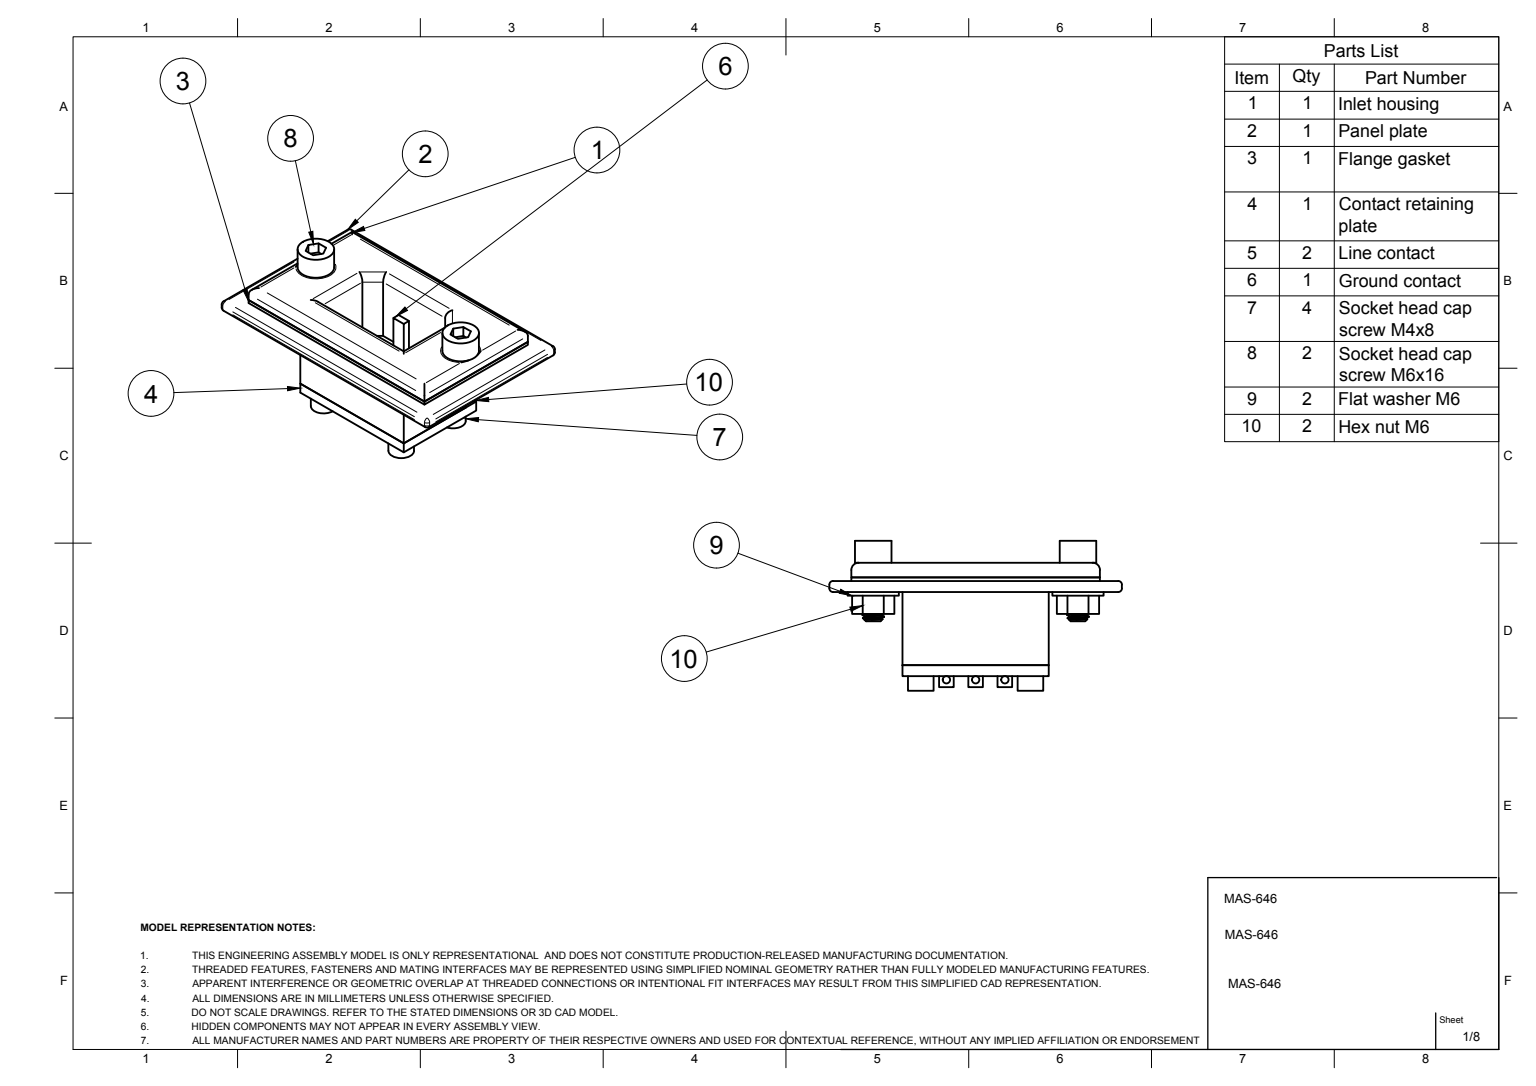
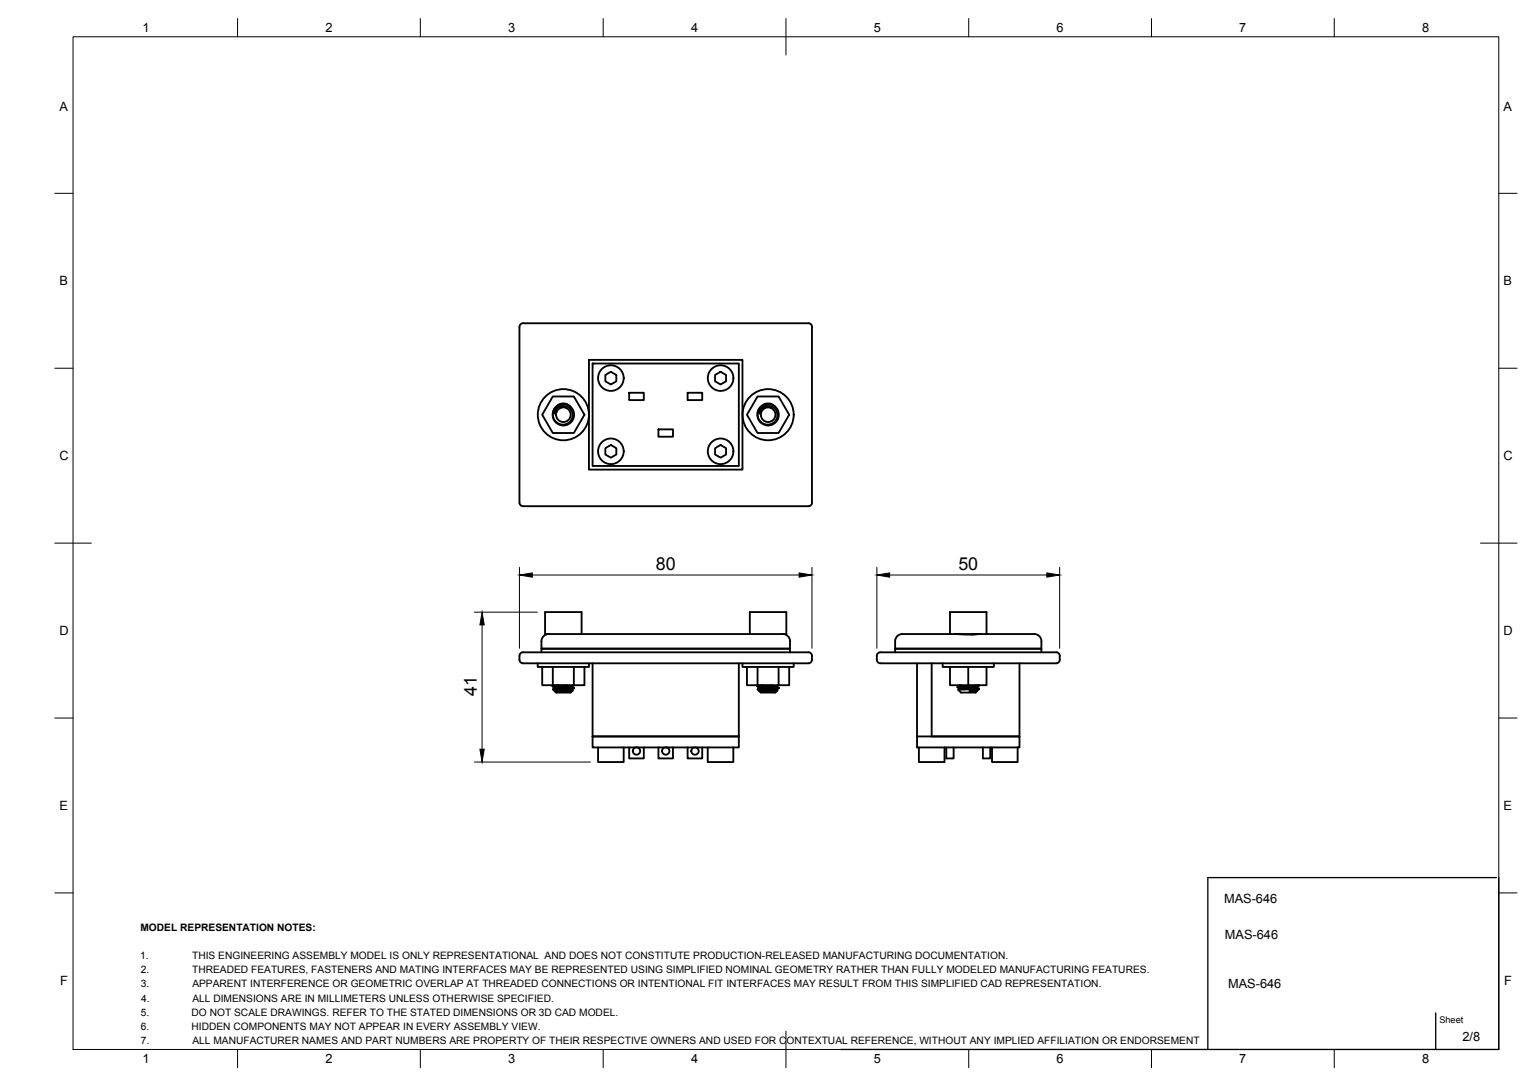
ISO-10303-21;
HEADER;
/* Generated by software containing ST-Developer
 * from STEP Tools, Inc. (www.steptools.com) 
 */

FILE_DESCRIPTION(
/* description */ ('Independent keyed three-contact power inlet for the IEC-connector des
ign category. Longer ground blade, retained contacts, wire termination
 holes and sealed bolted panel interface. Nominal custom interface; IE
C dimensional compatibility and electrical ratings are not assigned.'),

/* implementation_level */ '2;1');

FILE_NAME(
/* name */ 'MAS-646.step',
/* time_stamp */ '2026-11-08T19:55:04-08:00',
/* author */ (''),
/* organization */ (''),
/* preprocessor_version */ 'ST-DEVELOPER v20.2',
/* originating_system */ 'Autodesk Translation Framework v15.17.0.0',
/* authorisation */ '');

FILE_SCHEMA (('AUTOMOTIVE_DESIGN { 1 0 10303 214 3 1 1 }'));
ENDSEC;

DATA;
#10=MECHANICAL_DESIGN_GEOMETRIC_PRESENTATION_REPRESENTATION('',(#109,#110,
#111,#112,#113,#114,#115,#116,#117,#118),#21880);
#11=ITEM_DEFINED_TRANSFORMATION($,$,#6503,#6950);
#12=ITEM_DEFINED_TRANSFORMATION($,$,#6693,#6951);
#13=ITEM_DEFINED_TRANSFORMATION($,$,#6754,#6952);
#14=ITEM_DEFINED_TRANSFORMATION($,$,#6771,#6953);
#15=ITEM_DEFINED_TRANSFORMATION($,$,#6812,#6954);
#16=ITEM_DEFINED_TRANSFORMATION($,$,#6802,#6955);
#17=ITEM_DEFINED_TRANSFORMATION($,$,#6822,#6956);
#18=ITEM_DEFINED_TRANSFORMATION($,$,#6864,#6957);
#19=ITEM_DEFINED_TRANSFORMATION($,$,#6916,#6958);
#20=ITEM_DEFINED_TRANSFORMATION($,$,#6925,#6959);
#21=ITEM_DEFINED_TRANSFORMATION($,$,#6812,#6960);
#22=ITEM_DEFINED_TRANSFORMATION($,$,#6822,#6961);
#23=ITEM_DEFINED_TRANSFORMATION($,$,#6822,#6962);
#24=ITEM_DEFINED_TRANSFORMATION($,$,#6822,#6963);
#25=ITEM_DEFINED_TRANSFORMATION($,$,#6864,#6964);
#26=ITEM_DEFINED_TRANSFORMATION($,$,#6916,#6965);
#27=ITEM_DEFINED_TRANSFORMATION($,$,#6925,#6966);
#28=(
REPRESENTATION_RELATIONSHIP($,$,#21925,#21924)
REPRESENTATION_RELATIONSHIP_WITH_TRANSFORMATION(#11)
SHAPE_REPRESENTATION_RELATIONSHIP()
);
#29=(
REPRESENTATION_RELATIONSHIP($,$,#21926,#21924)
REPRESENTATION_RELATIONSHIP_WITH_TRANSFORMATION(#12)
SHAPE_REPRESENTATION_RELATIONSHIP()
);
#30=(
REPRESENTATION_RELATIONSHIP($,$,#21927,#21924)
REPRESENTATION_RELATIONSHIP_WITH_TRANSFORMATION(#13)
SHAPE_REPRESENTATION_RELATIONSHIP()
);
#31=(
REPRESENTATION_RELATIONSHIP($,$,#21928,#21924)
REPRESENTATION_RELATIONSHIP_WITH_TRANSFORMATION(#14)
SHAPE_REPRESENTATION_RELATIONSHIP()
);
#32=(
REPRESENTATION_RELATIONSHIP($,$,#21930,#21924)
REPRESENTATION_RELATIONSHIP_WITH_TRANSFORMATION(#15)
SHAPE_REPRESENTATION_RELATIONSHIP()
);
#33=(
REPRESENTATION_RELATIONSHIP($,$,#21929,#21924)
REPRESENTATION_RELATIONSHIP_WITH_TRANSFORMATION(#16)
SHAPE_REPRESENTATION_RELATIONSHIP()
);
#34=(
REPRESENTATION_RELATIONSHIP($,$,#21931,#21924)
REPRESENTATION_RELATIONSHIP_WITH_TRANSFORMATION(#17)
SHAPE_REPRESENTATION_RELATIONSHIP()
);
#35=(
REPRESENTATION_RELATIONSHIP($,$,#21932,#21924)
REPRESENTATION_RELATIONSHIP_WITH_TRANSFORMATION(#18)
SHAPE_REPRESENTATION_RELATIONSHIP()
);
#36=(
REPRESENTATION_RELATIONSHIP($,$,#21933,#21924)
REPRESENTATION_RELATIONSHIP_WITH_TRANSFORMATION(#19)
SHAPE_REPRESENTATION_RELATIONSHIP()
);
#37=(
REPRESENTATION_RELATIONSHIP($,$,#21934,#21924)
REPRESENTATION_RELATIONSHIP_WITH_TRANSFORMATION(#20)
SHAPE_REPRESENTATION_RELATIONSHIP()
);
#38=(
REPRESENTATION_RELATIONSHIP($,$,#21930,#21924)
REPRESENTATION_RELATIONSHIP_WITH_TRANSFORMATION(#21)
SHAPE_REPRESENTATION_RELATIONSHIP()
);
#39=(
REPRESENTATION_RELATIONSHIP($,$,#21931,#21924)
REPRESENTATION_RELATIONSHIP_WITH_TRANSFORMATION(#22)
SHAPE_REPRESENTATION_RELATIONSHIP()
);
#40=(
REPRESENTATION_RELATIONSHIP($,$,#21931,#21924)
REPRESENTATION_RELATIONSHIP_WITH_TRANSFORMATION(#23)
SHAPE_REPRESENTATION_RELATIONSHIP()
);
#41=(
REPRESENTATION_RELATIONSHIP($,$,#21931,#21924)
REPRESENTATION_RELATIONSHIP_WITH_TRANSFORMATION(#24)
SHAPE_REPRESENTATION_RELATIONSHIP()
);
#42=(
REPRESENTATION_RELATIONSHIP($,$,#21932,#21924)
REPRESENTATION_RELATIONSHIP_WITH_TRANSFORMATION(#25)
SHAPE_REPRESENTATION_RELATIONSHIP()
);
#43=(
REPRESENTATION_RELATIONSHIP($,$,#21933,#21924)
REPRESENTATION_RELATIONSHIP_WITH_TRANSFORMATION(#26)
SHAPE_REPRESENTATION_RELATIONSHIP()
);
#44=(
REPRESENTATION_RELATIONSHIP($,$,#21934,#21924)
REPRESENTATION_RELATIONSHIP_WITH_TRANSFORMATION(#27)
SHAPE_REPRESENTATION_RELATIONSHIP()
);
#45=CONTEXT_DEPENDENT_SHAPE_REPRESENTATION(#28,#21907);
#46=CONTEXT_DEPENDENT_SHAPE_REPRESENTATION(#29,#21908);
#47=CONTEXT_DEPENDENT_SHAPE_REPRESENTATION(#30,#21909);
#48=CONTEXT_DEPENDENT_SHAPE_REPRESENTATION(#31,#21910);
#49=CONTEXT_DEPENDENT_SHAPE_REPRESENTATION(#32,#21911);
#50=CONTEXT_DEPENDENT_SHAPE_REPRESENTATION(#33,#21912);
#51=CONTEXT_DEPENDENT_SHAPE_REPRESENTATION(#34,#21913);
#52=CONTEXT_DEPENDENT_SHAPE_REPRESENTATION(#35,#21914);
#53=CONTEXT_DEPENDENT_SHAPE_REPRESENTATION(#36,#21915);
#54=CONTEXT_DEPENDENT_SHAPE_REPRESENTATION(#37,#21916);
#55=CONTEXT_DEPENDENT_SHAPE_REPRESENTATION(#38,#21917);
#56=CONTEXT_DEPENDENT_SHAPE_REPRESENTATION(#39,#21918);
#57=CONTEXT_DEPENDENT_SHAPE_REPRESENTATION(#40,#21919);
#58=CONTEXT_DEPENDENT_SHAPE_REPRESENTATION(#41,#21920);
#59=CONTEXT_DEPENDENT_SHAPE_REPRESENTATION(#42,#21921);
#60=CONTEXT_DEPENDENT_SHAPE_REPRESENTATION(#43,#21922);
#61=CONTEXT_DEPENDENT_SHAPE_REPRESENTATION(#44,#21923);
#62=NEXT_ASSEMBLY_USAGE_OCCURRENCE('Inlet housing:1','Inlet housing:1',
'Inlet housing:1',#21936,#21937,'Inlet housing:1');
#63=NEXT_ASSEMBLY_USAGE_OCCURRENCE('Panel plate:1','Panel plate:1',
'Panel plate:1',#21936,#21938,'Panel plate:1');
#64=NEXT_ASSEMBLY_USAGE_OCCURRENCE('Flange gasket:1','Flange gasket:1',
'Flange gasket:1',#21936,#21939,'Flange gasket:1');
#65=NEXT_ASSEMBLY_USAGE_OCCURRENCE('Contact retaining plate:1',
'Contact retaining plate:1','Contact retaining plate:1',#21936,#21940,
'Contact retaining plate:1');
#66=NEXT_ASSEMBLY_USAGE_OCCURRENCE('Line contact:1','Line contact:1',
'Line contact:1',#21936,#21942,'Line contact:1');
#67=NEXT_ASSEMBLY_USAGE_OCCURRENCE('Ground contact:1',
'Ground contact:1','Ground contact:1',#21936,#21941,'Ground contact:1');
#68=NEXT_ASSEMBLY_USAGE_OCCURRENCE('Socket head cap screw M4x8:1',
'Socket head cap screw M4x8:1','Socket head cap screw M4x8:1',#21936,#21943,
'Socket head cap screw M4x8:1');
#69=NEXT_ASSEMBLY_USAGE_OCCURRENCE('Socket head cap screw M6x16:1',
'Socket head cap screw M6x16:1','Socket head cap screw M6x16:1',#21936,
#21944,'Socket head cap screw M6x16:1');
#70=NEXT_ASSEMBLY_USAGE_OCCURRENCE('Flat washer M6:1',
'Flat washer M6:1','Flat washer M6:1',#21936,#21945,'Flat washer M6:1');
#71=NEXT_ASSEMBLY_USAGE_OCCURRENCE('Hex nut M6:1','Hex nut M6:1',
'Hex nut M6:1',#21936,#21946,'Hex nut M6:1');
#72=NEXT_ASSEMBLY_USAGE_OCCURRENCE('Line contact:2','Line contact:2',
'Line contact:2',#21936,#21942,'Line contact:2');
#73=NEXT_ASSEMBLY_USAGE_OCCURRENCE('Socket head cap screw M4x8:2',
'Socket head cap screw M4x8:2','Socket head cap screw M4x8:2',#21936,#21943,
'Socket head cap screw M4x8:2');
#74=NEXT_ASSEMBLY_USAGE_OCCURRENCE('Socket head cap screw M4x8:3',
'Socket head cap screw M4x8:3','Socket head cap screw M4x8:3',#21936,#21943,
'Socket head cap screw M4x8:3');
#75=NEXT_ASSEMBLY_USAGE_OCCURRENCE('Socket head cap screw M4x8:4',
'Socket head cap screw M4x8:4','Socket head cap screw M4x8:4',#21936,#21943,
'Socket head cap screw M4x8:4');
#76=NEXT_ASSEMBLY_USAGE_OCCURRENCE('Socket head cap screw M6x16:2',
'Socket head cap screw M6x16:2','Socket head cap screw M6x16:2',#21936,
#21944,'Socket head cap screw M6x16:2');
#77=NEXT_ASSEMBLY_USAGE_OCCURRENCE('Flat washer M6:2',
'Flat washer M6:2','Flat washer M6:2',#21936,#21945,'Flat washer M6:2');
#78=NEXT_ASSEMBLY_USAGE_OCCURRENCE('Hex nut M6:2','Hex nut M6:2',
'Hex nut M6:2',#21936,#21946,'Hex nut M6:2');
#79=CONICAL_SURFACE('',#6845,1.5,0.785398163397448);
#80=CONICAL_SURFACE('',#6897,2.5,0.785398163397448);
#81=SPHERICAL_SURFACE('',#6694,0.999999999999996);
#82=SPHERICAL_SURFACE('',#6698,0.999999999999996);
#83=SPHERICAL_SURFACE('',#6702,1.);
#84=SPHERICAL_SURFACE('',#6706,0.999999999999996);
#85=SPHERICAL_SURFACE('',#6710,1.);
#86=SPHERICAL_SURFACE('',#6714,0.999999999999996);
#87=SPHERICAL_SURFACE('',#6718,1.);
#88=SPHERICAL_SURFACE('',#6722,1.);
#89=SHAPE_REPRESENTATION_RELATIONSHIP('SRR','None',#21925,#99);
#90=SHAPE_REPRESENTATION_RELATIONSHIP('SRR','None',#21926,#100);
#91=SHAPE_REPRESENTATION_RELATIONSHIP('SRR','None',#21927,#101);
#92=SHAPE_REPRESENTATION_RELATIONSHIP('SRR','None',#21928,#102);
#93=SHAPE_REPRESENTATION_RELATIONSHIP('SRR','None',#21929,#103);
#94=SHAPE_REPRESENTATION_RELATIONSHIP('SRR','None',#21930,#104);
#95=SHAPE_REPRESENTATION_RELATIONSHIP('SRR','None',#21931,#105);
#96=SHAPE_REPRESENTATION_RELATIONSHIP('SRR','None',#21932,#106);
#97=SHAPE_REPRESENTATION_RELATIONSHIP('SRR','None',#21933,#107);
#98=SHAPE_REPRESENTATION_RELATIONSHIP('SRR','None',#21934,#108);
#99=ADVANCED_BREP_SHAPE_REPRESENTATION('',(#119),#21870);
#100=ADVANCED_BREP_SHAPE_REPRESENTATION('',(#120),#21871);
#101=ADVANCED_BREP_SHAPE_REPRESENTATION('',(#121),#21872);
#102=ADVANCED_BREP_SHAPE_REPRESENTATION('',(#122),#21873);
#103=ADVANCED_BREP_SHAPE_REPRESENTATION('',(#123),#21874);
#104=ADVANCED_BREP_SHAPE_REPRESENTATION('',(#124),#21875);
#105=ADVANCED_BREP_SHAPE_REPRESENTATION('',(#125),#21876);
#106=ADVANCED_BREP_SHAPE_REPRESENTATION('',(#126),#21877);
#107=ADVANCED_BREP_SHAPE_REPRESENTATION('',(#127),#21878);
#108=ADVANCED_BREP_SHAPE_REPRESENTATION('',(#128),#21879);
#109=STYLED_ITEM('',(#21984),#119);
#110=STYLED_ITEM('',(#21985),#120);
#111=STYLED_ITEM('',(#21986),#121);
#112=STYLED_ITEM('',(#21987),#122);
#113=STYLED_ITEM('',(#21988),#123);
#114=STYLED_ITEM('',(#21988),#124);
#115=STYLED_ITEM('',(#21986),#125);
#116=STYLED_ITEM('',(#21986),#126);
#117=STYLED_ITEM('',(#21988),#127);
#118=STYLED_ITEM('',(#21985),#128);
#119=MANIFOLD_SOLID_BREP('Body1',#6381);
#120=MANIFOLD_SOLID_BREP('Body1',#6382);
#121=MANIFOLD_SOLID_BREP('Body1',#6383);
#122=MANIFOLD_SOLID_BREP('Body1',#6384);
#123=MANIFOLD_SOLID_BREP('Body1',#6385);
#124=MANIFOLD_SOLID_BREP('Body1',#6386);
#125=MANIFOLD_SOLID_BREP('Body1',#6387);
#126=MANIFOLD_SOLID_BREP('Body1',#6388);
#127=MANIFOLD_SOLID_BREP('Body1',#6389);
#128=MANIFOLD_SOLID_BREP('Body1',#6390);
#129=B_SPLINE_SURFACE_WITH_KNOTS('',3,3,((#11744,#11745,#11746,#11747,#11748,
#11749,#11750,#11751,#11752,#11753,#11754,#11755,#11756,#11757,#11758,#11759,
#11760,#11761,#11762,#11763,#11764,#11765,#11766,#11767,#11768,#11769,#11770,
#11771,#11772,#11773,#11774,#11775,#11776,#11777,#11778,#11779,#11780,#11781,
#11782,#11783,#11784,#11785,#11786,#11787,#11788,#11789,#11790,#11791,#11792,
#11793,#11794,#11795,#11796,#11797,#11798,#11799,#11800,#11801,#11802,#11803,
#11804,#11805,#11806,#11807,#11808,#11809,#11810,#11811,#11812,#11813,#11814,
#11815,#11816,#11817,#11818,#11819,#11820),(#11821,#11822,#11823,#11824,
#11825,#11826,#11827,#11828,#11829,#11830,#11831,#11832,#11833,#11834,#11835,
#11836,#11837,#11838,#11839,#11840,#11841,#11842,#11843,#11844,#11845,#11846,
#11847,#11848,#11849,#11850,#11851,#11852,#11853,#11854,#11855,#11856,#11857,
#11858,#11859,#11860,#11861,#11862,#11863,#11864,#11865,#11866,#11867,#11868,
#11869,#11870,#11871,#11872,#11873,#11874,#11875,#11876,#11877,#11878,#11879,
#11880,#11881,#11882,#11883,#11884,#11885,#11886,#11887,#11888,#11889,#11890,
#11891,#11892,#11893,#11894,#11895,#11896,#11897),(#11898,#11899,#11900,
#11901,#11902,#11903,#11904,#11905,#11906,#11907,#11908,#11909,#11910,#11911,
#11912,#11913,#11914,#11915,#11916,#11917,#11918,#11919,#11920,#11921,#11922,
#11923,#11924,#11925,#11926,#11927,#11928,#11929,#11930,#11931,#11932,#11933,
#11934,#11935,#11936,#11937,#11938,#11939,#11940,#11941,#11942,#11943,#11944,
#11945,#11946,#11947,#11948,#11949,#11950,#11951,#11952,#11953,#11954,#11955,
#11956,#11957,#11958,#11959,#11960,#11961,#11962,#11963,#11964,#11965,#11966,
#11967,#11968,#11969,#11970,#11971,#11972,#11973,#11974),(#11975,#11976,
#11977,#11978,#11979,#11980,#11981,#11982,#11983,#11984,#11985,#11986,#11987,
#11988,#11989,#11990,#11991,#11992,#11993,#11994,#11995,#11996,#11997,#11998,
#11999,#12000,#12001,#12002,#12003,#12004,#12005,#12006,#12007,#12008,#12009,
#12010,#12011,#12012,#12013,#12014,#12015,#12016,#12017,#12018,#12019,#12020,
#12021,#12022,#12023,#12024,#12025,#12026,#12027,#12028,#12029,#12030,#12031,
#12032,#12033,#12034,#12035,#12036,#12037,#12038,#12039,#12040,#12041,#12042,
#12043,#12044,#12045,#12046,#12047,#12048,#12049,#12050,#12051)),
 .UNSPECIFIED.,.F.,.F.,.F.,(4,4),(4,1,1,1,1,1,1,1,1,1,1,1,1,1,1,1,1,1,1,
1,1,1,1,1,1,1,1,1,1,1,1,1,1,1,1,1,1,1,1,1,1,1,1,1,1,1,1,1,1,1,1,1,1,1,1,
1,1,1,1,1,1,1,1,1,1,1,1,1,1,1,1,1,1,1,4),(0.,0.0448889834294934),(11.8615800042567,
12.859180611653,13.8567812190493,14.8543818264456,15.8519824338419,16.8495830412382,
17.8471836486345,18.8447842560309,19.8423848634272,20.8399854708235,21.8375860782198,
22.8351866856161,23.8327872930124,24.8303879004087,25.827988507805,26.8255891152013,
27.8231897225976,28.8207903299939,29.8183909373903,30.8159915447866,31.8135921521829,
32.8111927595792,33.8087933669755,34.8063939743718,35.8039945817681,36.8015951891644,
37.7991957965607,38.796796403957,39.7943970113533,40.7919976187497,41.789598226146,
42.7871988335423,43.7847994409386,44.7824000483349,45.7800006557312,46.7776012631275,
47.7752018705238,48.7728024779201,49.7704030853164,50.7680036927128,51.7656043001091,
52.7632049075054,53.7608055149017,54.758406122298,55.7560067296943,56.7536073370906,
57.7512079444869,58.7488085518832,59.7464091592795,60.7440097666758,61.7416103740722,
62.7392109814685,63.7368115888648,64.7344121962611,65.7320128036574,66.7296134110537,
67.72721401845,68.7248146258463,69.7224152332426,70.7200158406389,71.7176164480352,
72.7152170554316,73.7128176628279,74.7104182702242,75.7080188776205,76.7056194850168,
77.7032200924131,78.7008206998094,79.6984213072057,80.696021914602,81.6936225219983,
82.6912231293946,83.688823736791,84.6864243441873,85.6840249515836),
 .UNSPECIFIED.);
#130=B_SPLINE_SURFACE_WITH_KNOTS('',3,3,((#12248,#12249,#12250,#12251,#12252,
#12253,#12254,#12255,#12256,#12257,#12258,#12259,#12260,#12261,#12262,#12263,
#12264,#12265,#12266,#12267,#12268,#12269,#12270,#12271,#12272,#12273,#12274,
#12275,#12276,#12277,#12278,#12279,#12280,#12281,#12282,#12283,#12284,#12285,
#12286,#12287,#12288,#12289,#12290,#12291,#12292,#12293,#12294,#12295,#12296,
#12297,#12298,#12299,#12300,#12301,#12302,#12303,#12304,#12305,#12306,#12307,
#12308,#12309,#12310,#12311,#12312,#12313,#12314,#12315,#12316,#12317,#12318,
#12319,#12320,#12321,#12322,#12323,#12324),(#12325,#12326,#12327,#12328,
#12329,#12330,#12331,#12332,#12333,#12334,#12335,#12336,#12337,#12338,#12339,
#12340,#12341,#12342,#12343,#12344,#12345,#12346,#12347,#12348,#12349,#12350,
#12351,#12352,#12353,#12354,#12355,#12356,#12357,#12358,#12359,#12360,#12361,
#12362,#12363,#12364,#12365,#12366,#12367,#12368,#12369,#12370,#12371,#12372,
#12373,#12374,#12375,#12376,#12377,#12378,#12379,#12380,#12381,#12382,#12383,
#12384,#12385,#12386,#12387,#12388,#12389,#12390,#12391,#12392,#12393,#12394,
#12395,#12396,#12397,#12398,#12399,#12400,#12401),(#12402,#12403,#12404,
#12405,#12406,#12407,#12408,#12409,#12410,#12411,#12412,#12413,#12414,#12415,
#12416,#12417,#12418,#12419,#12420,#12421,#12422,#12423,#12424,#12425,#12426,
#12427,#12428,#12429,#12430,#12431,#12432,#12433,#12434,#12435,#12436,#12437,
#12438,#12439,#12440,#12441,#12442,#12443,#12444,#12445,#12446,#12447,#12448,
#12449,#12450,#12451,#12452,#12453,#12454,#12455,#12456,#12457,#12458,#12459,
#12460,#12461,#12462,#12463,#12464,#12465,#12466,#12467,#12468,#12469,#12470,
#12471,#12472,#12473,#12474,#12475,#12476,#12477,#12478),(#12479,#12480,
#12481,#12482,#12483,#12484,#12485,#12486,#12487,#12488,#12489,#12490,#12491,
#12492,#12493,#12494,#12495,#12496,#12497,#12498,#12499,#12500,#12501,#12502,
#12503,#12504,#12505,#12506,#12507,#12508,#12509,#12510,#12511,#12512,#12513,
#12514,#12515,#12516,#12517,#12518,#12519,#12520,#12521,#12522,#12523,#12524,
#12525,#12526,#12527,#12528,#12529,#12530,#12531,#12532,#12533,#12534,#12535,
#12536,#12537,#12538,#12539,#12540,#12541,#12542,#12543,#12544,#12545,#12546,
#12547,#12548,#12549,#12550,#12551,#12552,#12553,#12554,#12555)),
 .UNSPECIFIED.,.F.,.F.,.F.,(4,4),(4,1,1,1,1,1,1,1,1,1,1,1,1,1,1,1,1,1,1,
1,1,1,1,1,1,1,1,1,1,1,1,1,1,1,1,1,1,1,1,1,1,1,1,1,1,1,1,1,1,1,1,1,1,1,1,
1,1,1,1,1,1,1,1,1,1,1,1,1,1,1,1,1,1,1,4),(0.,0.0448889834294934),(14.3981410127769,
15.3957416201732,16.3933422275696,17.3909428349659,18.3885434423622,19.3861440497585,
20.3837446571548,21.3813452645511,22.3789458719474,23.3765464793437,24.37414708674,
25.3717476941363,26.3693483015326,27.366948908929,28.3645495163253,29.3621501237216,
30.3597507311179,31.3573513385142,32.3549519459105,33.3525525533068,34.3501531607031,
35.3477537680994,36.3453543754957,37.342954982892,38.3405555902884,39.3381561976847,
40.335756805081,41.3333574124773,42.3309580198736,43.3285586272699,44.3261592346662,
45.3237598420625,46.3213604494588,47.3189610568551,48.3165616642514,49.3141622716478,
50.3117628790441,51.3093634864404,52.3069640938367,53.304564701233,54.3021653086293,
55.2997659160256,56.2973665234219,57.2949671308182,58.2925677382145,59.2901683456108,
60.2877689530072,61.2853695604035,62.2829701677998,63.2805707751961,64.2781713825924,
65.2757719899887,66.273372597385,67.2709732047813,68.2685738121776,69.2661744195739,
70.2637750269702,71.2613756343666,72.2589762417629,73.2565768491592,74.2541774565555,
75.2517780639518,76.2493786713481,77.2469792787444,78.2445798861407,79.242180493537,
80.2397811009333,81.2373817083296,82.2349823157259,83.2325829231223,84.2301835305186,
85.2277841379149,86.2253847453112,87.2229853527075,88.2205859601038),
 .UNSPECIFIED.);
#131=B_SPLINE_SURFACE_WITH_KNOTS('',3,3,((#13305,#13306,#13307,#13308,#13309,
#13310,#13311,#13312,#13313,#13314,#13315,#13316,#13317,#13318,#13319,#13320,
#13321,#13322,#13323,#13324,#13325,#13326,#13327,#13328,#13329,#13330,#13331,
#13332,#13333,#13334,#13335,#13336,#13337,#13338,#13339,#13340,#13341,#13342,
#13343,#13344,#13345,#13346,#13347,#13348,#13349,#13350,#13351,#13352,#13353,
#13354,#13355,#13356,#13357,#13358,#13359,#13360,#13361,#13362,#13363,#13364,
#13365,#13366,#13367,#13368,#13369,#13370,#13371,#13372,#13373,#13374,#13375,
#13376,#13377,#13378,#13379,#13380,#13381),(#13382,#13383,#13384,#13385,
#13386,#13387,#13388,#13389,#13390,#13391,#13392,#13393,#13394,#13395,#13396,
#13397,#13398,#13399,#13400,#13401,#13402,#13403,#13404,#13405,#13406,#13407,
#13408,#13409,#13410,#13411,#13412,#13413,#13414,#13415,#13416,#13417,#13418,
#13419,#13420,#13421,#13422,#13423,#13424,#13425,#13426,#13427,#13428,#13429,
#13430,#13431,#13432,#13433,#13434,#13435,#13436,#13437,#13438,#13439,#13440,
#13441,#13442,#13443,#13444,#13445,#13446,#13447,#13448,#13449,#13450,#13451,
#13452,#13453,#13454,#13455,#13456,#13457,#13458),(#13459,#13460,#13461,
#13462,#13463,#13464,#13465,#13466,#13467,#13468,#13469,#13470,#13471,#13472,
#13473,#13474,#13475,#13476,#13477,#13478,#13479,#13480,#13481,#13482,#13483,
#13484,#13485,#13486,#13487,#13488,#13489,#13490,#13491,#13492,#13493,#13494,
#13495,#13496,#13497,#13498,#13499,#13500,#13501,#13502,#13503,#13504,#13505,
#13506,#13507,#13508,#13509,#13510,#13511,#13512,#13513,#13514,#13515,#13516,
#13517,#13518,#13519,#13520,#13521,#13522,#13523,#13524,#13525,#13526,#13527,
#13528,#13529,#13530,#13531,#13532,#13533,#13534,#13535),(#13536,#13537,
#13538,#13539,#13540,#13541,#13542,#13543,#13544,#13545,#13546,#13547,#13548,
#13549,#13550,#13551,#13552,#13553,#13554,#13555,#13556,#13557,#13558,#13559,
#13560,#13561,#13562,#13563,#13564,#13565,#13566,#13567,#13568,#13569,#13570,
#13571,#13572,#13573,#13574,#13575,#13576,#13577,#13578,#13579,#13580,#13581,
#13582,#13583,#13584,#13585,#13586,#13587,#13588,#13589,#13590,#13591,#13592,
#13593,#13594,#13595,#13596,#13597,#13598,#13599,#13600,#13601,#13602,#13603,
#13604,#13605,#13606,#13607,#13608,#13609,#13610,#13611,#13612)),
 .UNSPECIFIED.,.F.,.F.,.F.,(4,4),(4,1,1,1,1,1,1,1,1,1,1,1,1,1,1,1,1,1,1,
1,1,1,1,1,1,1,1,1,1,1,1,1,1,1,1,1,1,1,1,1,1,1,1,1,1,1,1,1,1,1,1,1,1,1,1,
1,1,1,1,1,1,1,1,1,1,1,1,1,1,1,1,1,1,1,4),(0.,0.0448889834294934),(11.8615800042567,
12.859180611653,13.8567812190493,14.8543818264456,15.8519824338419,16.8495830412382,
17.8471836486345,18.8447842560308,19.8423848634271,20.8399854708235,21.8375860782198,
22.8351866856161,23.8327872930124,24.8303879004087,25.827988507805,26.8255891152013,
27.8231897225976,28.8207903299939,29.8183909373902,30.8159915447865,31.8135921521829,
32.8111927595792,33.8087933669755,34.8063939743718,35.8039945817681,36.8015951891644,
37.7991957965607,38.796796403957,39.7943970113533,40.7919976187496,41.7895982261459,
42.7871988335423,43.7847994409386,44.7824000483349,45.7800006557312,46.7776012631275,
47.7752018705238,48.7728024779201,49.7704030853164,50.7680036927127,51.765604300109,
52.7632049075054,53.7608055149017,54.758406122298,55.7560067296943,56.7536073370906,
57.7512079444869,58.7488085518832,59.7464091592795,60.7440097666758,61.7416103740721,
62.7392109814684,63.7368115888648,64.7344121962611,65.7320128036574,66.7296134110537,
67.72721401845,68.7248146258463,69.7224152332426,70.7200158406389,71.7176164480352,
72.7152170554315,73.7128176628278,74.7104182702242,75.7080188776205,76.7056194850168,
77.7032200924131,78.7008206998094,79.6984213072057,80.696021914602,81.6936225219983,
82.6912231293946,83.6888237367909,84.6864243441872,85.6840249515836),
 .UNSPECIFIED.);
#132=B_SPLINE_SURFACE_WITH_KNOTS('',3,3,((#13726,#13727,#13728,#13729,#13730,
#13731,#13732,#13733,#13734,#13735,#13736,#13737,#13738,#13739,#13740,#13741,
#13742,#13743,#13744,#13745,#13746,#13747,#13748,#13749,#13750,#13751,#13752,
#13753,#13754,#13755,#13756,#13757,#13758,#13759,#13760,#13761,#13762,#13763,
#13764,#13765,#13766,#13767,#13768,#13769,#13770,#13771,#13772,#13773,#13774,
#13775,#13776,#13777,#13778,#13779,#13780,#13781,#13782,#13783,#13784,#13785,
#13786,#13787,#13788,#13789,#13790,#13791,#13792,#13793,#13794,#13795,#13796,
#13797,#13798,#13799,#13800,#13801,#13802),(#13803,#13804,#13805,#13806,
#13807,#13808,#13809,#13810,#13811,#13812,#13813,#13814,#13815,#13816,#13817,
#13818,#13819,#13820,#13821,#13822,#13823,#13824,#13825,#13826,#13827,#13828,
#13829,#13830,#13831,#13832,#13833,#13834,#13835,#13836,#13837,#13838,#13839,
#13840,#13841,#13842,#13843,#13844,#13845,#13846,#13847,#13848,#13849,#13850,
#13851,#13852,#13853,#13854,#13855,#13856,#13857,#13858,#13859,#13860,#13861,
#13862,#13863,#13864,#13865,#13866,#13867,#13868,#13869,#13870,#13871,#13872,
#13873,#13874,#13875,#13876,#13877,#13878,#13879),(#13880,#13881,#13882,
#13883,#13884,#13885,#13886,#13887,#13888,#13889,#13890,#13891,#13892,#13893,
#13894,#13895,#13896,#13897,#13898,#13899,#13900,#13901,#13902,#13903,#13904,
#13905,#13906,#13907,#13908,#13909,#13910,#13911,#13912,#13913,#13914,#13915,
#13916,#13917,#13918,#13919,#13920,#13921,#13922,#13923,#13924,#13925,#13926,
#13927,#13928,#13929,#13930,#13931,#13932,#13933,#13934,#13935,#13936,#13937,
#13938,#13939,#13940,#13941,#13942,#13943,#13944,#13945,#13946,#13947,#13948,
#13949,#13950,#13951,#13952,#13953,#13954,#13955,#13956),(#13957,#13958,
#13959,#13960,#13961,#13962,#13963,#13964,#13965,#13966,#13967,#13968,#13969,
#13970,#13971,#13972,#13973,#13974,#13975,#13976,#13977,#13978,#13979,#13980,
#13981,#13982,#13983,#13984,#13985,#13986,#13987,#13988,#13989,#13990,#13991,
#13992,#13993,#13994,#13995,#13996,#13997,#13998,#13999,#14000,#14001,#14002,
#14003,#14004,#14005,#14006,#14007,#14008,#14009,#14010,#14011,#14012,#14013,
#14014,#14015,#14016,#14017,#14018,#14019,#14020,#14021,#14022,#14023,#14024,
#14025,#14026,#14027,#14028,#14029,#14030,#14031,#14032,#14033)),
 .UNSPECIFIED.,.F.,.F.,.F.,(4,4),(4,1,1,1,1,1,1,1,1,1,1,1,1,1,1,1,1,1,1,
1,1,1,1,1,1,1,1,1,1,1,1,1,1,1,1,1,1,1,1,1,1,1,1,1,1,1,1,1,1,1,1,1,1,1,1,
1,1,1,1,1,1,1,1,1,1,1,1,1,1,1,1,1,1,1,4),(0.,0.0448889834294934),(14.3981410127769,
15.3957416201732,16.3933422275695,17.3909428349659,18.3885434423622,19.3861440497585,
20.3837446571548,21.3813452645511,22.3789458719474,23.3765464793437,24.37414708674,
25.3717476941363,26.3693483015326,27.3669489089289,28.3645495163252,29.3621501237216,
30.3597507311179,31.3573513385142,32.3549519459105,33.3525525533068,34.3501531607031,
35.3477537680994,36.3453543754957,37.342954982892,38.3405555902883,39.3381561976846,
40.335756805081,41.3333574124773,42.3309580198736,43.3285586272699,44.3261592346662,
45.3237598420625,46.3213604494588,47.3189610568551,48.3165616642514,49.3141622716477,
50.3117628790441,51.3093634864404,52.3069640938367,53.304564701233,54.3021653086293,
55.2997659160256,56.2973665234219,57.2949671308182,58.2925677382145,59.2901683456108,
60.2877689530071,61.2853695604035,62.2829701677998,63.2805707751961,64.2781713825924,
65.2757719899887,66.273372597385,67.2709732047813,68.2685738121776,69.2661744195739,
70.2637750269702,71.2613756343665,72.2589762417629,73.2565768491592,74.2541774565555,
75.2517780639518,76.2493786713481,77.2469792787444,78.2445798861407,79.242180493537,
80.2397811009333,81.2373817083296,82.2349823157259,83.2325829231222,84.2301835305186,
85.2277841379149,86.2253847453112,87.2229853527075,88.2205859601038),
 .UNSPECIFIED.);
#133=B_SPLINE_SURFACE_WITH_KNOTS('',3,3,((#14163,#14164,#14165,#14166,#14167,
#14168,#14169,#14170,#14171,#14172,#14173,#14174,#14175,#14176,#14177,#14178,
#14179,#14180,#14181,#14182,#14183,#14184,#14185,#14186,#14187,#14188,#14189,
#14190,#14191,#14192,#14193,#14194,#14195,#14196,#14197,#14198,#14199,#14200,
#14201,#14202,#14203,#14204,#14205,#14206,#14207,#14208,#14209,#14210,#14211,
#14212,#14213,#14214,#14215,#14216,#14217,#14218,#14219,#14220,#14221,#14222,
#14223,#14224,#14225,#14226,#14227,#14228,#14229,#14230,#14231,#14232,#14233,
#14234,#14235,#14236,#14237,#14238,#14239),(#14240,#14241,#14242,#14243,
#14244,#14245,#14246,#14247,#14248,#14249,#14250,#14251,#14252,#14253,#14254,
#14255,#14256,#14257,#14258,#14259,#14260,#14261,#14262,#14263,#14264,#14265,
#14266,#14267,#14268,#14269,#14270,#14271,#14272,#14273,#14274,#14275,#14276,
#14277,#14278,#14279,#14280,#14281,#14282,#14283,#14284,#14285,#14286,#14287,
#14288,#14289,#14290,#14291,#14292,#14293,#14294,#14295,#14296,#14297,#14298,
#14299,#14300,#14301,#14302,#14303,#14304,#14305,#14306,#14307,#14308,#14309,
#14310,#14311,#14312,#14313,#14314,#14315,#14316),(#14317,#14318,#14319,
#14320,#14321,#14322,#14323,#14324,#14325,#14326,#14327,#14328,#14329,#14330,
#14331,#14332,#14333,#14334,#14335,#14336,#14337,#14338,#14339,#14340,#14341,
#14342,#14343,#14344,#14345,#14346,#14347,#14348,#14349,#14350,#14351,#14352,
#14353,#14354,#14355,#14356,#14357,#14358,#14359,#14360,#14361,#14362,#14363,
#14364,#14365,#14366,#14367,#14368,#14369,#14370,#14371,#14372,#14373,#14374,
#14375,#14376,#14377,#14378,#14379,#14380,#14381,#14382,#14383,#14384,#14385,
#14386,#14387,#14388,#14389,#14390,#14391,#14392,#14393),(#14394,#14395,
#14396,#14397,#14398,#14399,#14400,#14401,#14402,#14403,#14404,#14405,#14406,
#14407,#14408,#14409,#14410,#14411,#14412,#14413,#14414,#14415,#14416,#14417,
#14418,#14419,#14420,#14421,#14422,#14423,#14424,#14425,#14426,#14427,#14428,
#14429,#14430,#14431,#14432,#14433,#14434,#14435,#14436,#14437,#14438,#14439,
#14440,#14441,#14442,#14443,#14444,#14445,#14446,#14447,#14448,#14449,#14450,
#14451,#14452,#14453,#14454,#14455,#14456,#14457,#14458,#14459,#14460,#14461,
#14462,#14463,#14464,#14465,#14466,#14467,#14468,#14469,#14470)),
 .UNSPECIFIED.,.F.,.F.,.F.,(4,4),(4,1,1,1,1,1,1,1,1,1,1,1,1,1,1,1,1,1,1,
1,1,1,1,1,1,1,1,1,1,1,1,1,1,1,1,1,1,1,1,1,1,1,1,1,1,1,1,1,1,1,1,1,1,1,1,
1,1,1,1,1,1,1,1,1,1,1,1,1,1,1,1,1,1,1,4),(0.,0.0448889834294934),(11.8615800042567,
12.859180611653,13.8567812190493,14.8543818264456,15.8519824338419,16.8495830412382,
17.8471836486345,18.8447842560308,19.8423848634271,20.8399854708235,21.8375860782198,
22.8351866856161,23.8327872930124,24.8303879004087,25.827988507805,26.8255891152013,
27.8231897225976,28.8207903299939,29.8183909373902,30.8159915447865,31.8135921521829,
32.8111927595792,33.8087933669755,34.8063939743718,35.8039945817681,36.8015951891644,
37.7991957965607,38.796796403957,39.7943970113533,40.7919976187496,41.7895982261459,
42.7871988335423,43.7847994409386,44.7824000483349,45.7800006557312,46.7776012631275,
47.7752018705238,48.7728024779201,49.7704030853164,50.7680036927127,51.765604300109,
52.7632049075054,53.7608055149017,54.758406122298,55.7560067296943,56.7536073370906,
57.7512079444869,58.7488085518832,59.7464091592795,60.7440097666758,61.7416103740721,
62.7392109814684,63.7368115888648,64.7344121962611,65.7320128036574,66.7296134110537,
67.72721401845,68.7248146258463,69.7224152332426,70.7200158406389,71.7176164480352,
72.7152170554315,73.7128176628278,74.7104182702242,75.7080188776205,76.7056194850168,
77.7032200924131,78.7008206998094,79.6984213072057,80.696021914602,81.6936225219983,
82.6912231293946,83.6888237367909,84.6864243441872,85.6840249515836),
 .UNSPECIFIED.);
#134=B_SPLINE_SURFACE_WITH_KNOTS('',3,3,((#14584,#14585,#14586,#14587,#14588,
#14589,#14590,#14591,#14592,#14593,#14594,#14595,#14596,#14597,#14598,#14599,
#14600,#14601,#14602,#14603,#14604,#14605,#14606,#14607,#14608,#14609,#14610,
#14611,#14612,#14613,#14614,#14615,#14616,#14617,#14618,#14619,#14620,#14621,
#14622,#14623,#14624,#14625,#14626,#14627,#14628,#14629,#14630,#14631,#14632,
#14633,#14634,#14635,#14636,#14637,#14638,#14639,#14640,#14641,#14642,#14643,
#14644,#14645,#14646,#14647,#14648,#14649,#14650,#14651,#14652,#14653,#14654,
#14655,#14656,#14657,#14658,#14659,#14660),(#14661,#14662,#14663,#14664,
#14665,#14666,#14667,#14668,#14669,#14670,#14671,#14672,#14673,#14674,#14675,
#14676,#14677,#14678,#14679,#14680,#14681,#14682,#14683,#14684,#14685,#14686,
#14687,#14688,#14689,#14690,#14691,#14692,#14693,#14694,#14695,#14696,#14697,
#14698,#14699,#14700,#14701,#14702,#14703,#14704,#14705,#14706,#14707,#14708,
#14709,#14710,#14711,#14712,#14713,#14714,#14715,#14716,#14717,#14718,#14719,
#14720,#14721,#14722,#14723,#14724,#14725,#14726,#14727,#14728,#14729,#14730,
#14731,#14732,#14733,#14734,#14735,#14736,#14737),(#14738,#14739,#14740,
#14741,#14742,#14743,#14744,#14745,#14746,#14747,#14748,#14749,#14750,#14751,
#14752,#14753,#14754,#14755,#14756,#14757,#14758,#14759,#14760,#14761,#14762,
#14763,#14764,#14765,#14766,#14767,#14768,#14769,#14770,#14771,#14772,#14773,
#14774,#14775,#14776,#14777,#14778,#14779,#14780,#14781,#14782,#14783,#14784,
#14785,#14786,#14787,#14788,#14789,#14790,#14791,#14792,#14793,#14794,#14795,
#14796,#14797,#14798,#14799,#14800,#14801,#14802,#14803,#14804,#14805,#14806,
#14807,#14808,#14809,#14810,#14811,#14812,#14813,#14814),(#14815,#14816,
#14817,#14818,#14819,#14820,#14821,#14822,#14823,#14824,#14825,#14826,#14827,
#14828,#14829,#14830,#14831,#14832,#14833,#14834,#14835,#14836,#14837,#14838,
#14839,#14840,#14841,#14842,#14843,#14844,#14845,#14846,#14847,#14848,#14849,
#14850,#14851,#14852,#14853,#14854,#14855,#14856,#14857,#14858,#14859,#14860,
#14861,#14862,#14863,#14864,#14865,#14866,#14867,#14868,#14869,#14870,#14871,
#14872,#14873,#14874,#14875,#14876,#14877,#14878,#14879,#14880,#14881,#14882,
#14883,#14884,#14885,#14886,#14887,#14888,#14889,#14890,#14891)),
 .UNSPECIFIED.,.F.,.F.,.F.,(4,4),(4,1,1,1,1,1,1,1,1,1,1,1,1,1,1,1,1,1,1,
1,1,1,1,1,1,1,1,1,1,1,1,1,1,1,1,1,1,1,1,1,1,1,1,1,1,1,1,1,1,1,1,1,1,1,1,
1,1,1,1,1,1,1,1,1,1,1,1,1,1,1,1,1,1,1,4),(0.,0.0448889834294934),(14.3981410127769,
15.3957416201732,16.3933422275695,17.3909428349659,18.3885434423622,19.3861440497585,
20.3837446571548,21.3813452645511,22.3789458719474,23.3765464793437,24.37414708674,
25.3717476941363,26.3693483015326,27.3669489089289,28.3645495163252,29.3621501237216,
30.3597507311179,31.3573513385142,32.3549519459105,33.3525525533068,34.3501531607031,
35.3477537680994,36.3453543754957,37.342954982892,38.3405555902883,39.3381561976846,
40.335756805081,41.3333574124773,42.3309580198736,43.3285586272699,44.3261592346662,
45.3237598420625,46.3213604494588,47.3189610568551,48.3165616642514,49.3141622716477,
50.3117628790441,51.3093634864404,52.3069640938367,53.304564701233,54.3021653086293,
55.2997659160256,56.2973665234219,57.2949671308182,58.2925677382145,59.2901683456108,
60.2877689530071,61.2853695604035,62.2829701677998,63.2805707751961,64.2781713825924,
65.2757719899887,66.273372597385,67.2709732047813,68.2685738121776,69.2661744195739,
70.2637750269702,71.2613756343665,72.2589762417629,73.2565768491592,74.2541774565555,
75.2517780639518,76.2493786713481,77.2469792787444,78.2445798861407,79.242180493537,
80.2397811009333,81.2373817083296,82.2349823157259,83.2325829231222,84.2301835305186,
85.2277841379149,86.2253847453112,87.2229853527075,88.2205859601038),
 .UNSPECIFIED.);
#135=B_SPLINE_SURFACE_WITH_KNOTS('',3,3,((#15021,#15022,#15023,#15024,#15025,
#15026,#15027,#15028,#15029,#15030,#15031,#15032,#15033,#15034,#15035,#15036,
#15037,#15038,#15039,#15040,#15041,#15042,#15043,#15044,#15045,#15046,#15047,
#15048,#15049,#15050,#15051,#15052,#15053,#15054,#15055,#15056,#15057,#15058,
#15059,#15060,#15061,#15062,#15063,#15064,#15065,#15066,#15067,#15068,#15069,
#15070,#15071,#15072,#15073,#15074,#15075,#15076,#15077,#15078,#15079,#15080,
#15081,#15082,#15083,#15084,#15085,#15086,#15087,#15088,#15089,#15090,#15091,
#15092,#15093,#15094,#15095,#15096,#15097),(#15098,#15099,#15100,#15101,
#15102,#15103,#15104,#15105,#15106,#15107,#15108,#15109,#15110,#15111,#15112,
#15113,#15114,#15115,#15116,#15117,#15118,#15119,#15120,#15121,#15122,#15123,
#15124,#15125,#15126,#15127,#15128,#15129,#15130,#15131,#15132,#15133,#15134,
#15135,#15136,#15137,#15138,#15139,#15140,#15141,#15142,#15143,#15144,#15145,
#15146,#15147,#15148,#15149,#15150,#15151,#15152,#15153,#15154,#15155,#15156,
#15157,#15158,#15159,#15160,#15161,#15162,#15163,#15164,#15165,#15166,#15167,
#15168,#15169,#15170,#15171,#15172,#15173,#15174),(#15175,#15176,#15177,
#15178,#15179,#15180,#15181,#15182,#15183,#15184,#15185,#15186,#15187,#15188,
#15189,#15190,#15191,#15192,#15193,#15194,#15195,#15196,#15197,#15198,#15199,
#15200,#15201,#15202,#15203,#15204,#15205,#15206,#15207,#15208,#15209,#15210,
#15211,#15212,#15213,#15214,#15215,#15216,#15217,#15218,#15219,#15220,#15221,
#15222,#15223,#15224,#15225,#15226,#15227,#15228,#15229,#15230,#15231,#15232,
#15233,#15234,#15235,#15236,#15237,#15238,#15239,#15240,#15241,#15242,#15243,
#15244,#15245,#15246,#15247,#15248,#15249,#15250,#15251),(#15252,#15253,
#15254,#15255,#15256,#15257,#15258,#15259,#15260,#15261,#15262,#15263,#15264,
#15265,#15266,#15267,#15268,#15269,#15270,#15271,#15272,#15273,#15274,#15275,
#15276,#15277,#15278,#15279,#15280,#15281,#15282,#15283,#15284,#15285,#15286,
#15287,#15288,#15289,#15290,#15291,#15292,#15293,#15294,#15295,#15296,#15297,
#15298,#15299,#15300,#15301,#15302,#15303,#15304,#15305,#15306,#15307,#15308,
#15309,#15310,#15311,#15312,#15313,#15314,#15315,#15316,#15317,#15318,#15319,
#15320,#15321,#15322,#15323,#15324,#15325,#15326,#15327,#15328)),
 .UNSPECIFIED.,.F.,.F.,.F.,(4,4),(4,1,1,1,1,1,1,1,1,1,1,1,1,1,1,1,1,1,1,
1,1,1,1,1,1,1,1,1,1,1,1,1,1,1,1,1,1,1,1,1,1,1,1,1,1,1,1,1,1,1,1,1,1,1,1,
1,1,1,1,1,1,1,1,1,1,1,1,1,1,1,1,1,1,1,4),(0.,0.0448889834294934),(11.8615800042567,
12.859180611653,13.8567812190493,14.8543818264456,15.8519824338419,16.8495830412382,
17.8471836486345,18.8447842560309,19.8423848634272,20.8399854708235,21.8375860782198,
22.8351866856161,23.8327872930124,24.8303879004087,25.827988507805,26.8255891152013,
27.8231897225976,28.8207903299939,29.8183909373903,30.8159915447866,31.8135921521829,
32.8111927595792,33.8087933669755,34.8063939743718,35.8039945817681,36.8015951891644,
37.7991957965607,38.796796403957,39.7943970113533,40.7919976187497,41.789598226146,
42.7871988335423,43.7847994409386,44.7824000483349,45.7800006557312,46.7776012631275,
47.7752018705238,48.7728024779201,49.7704030853164,50.7680036927127,51.7656043001091,
52.7632049075054,53.7608055149017,54.758406122298,55.7560067296943,56.7536073370906,
57.7512079444869,58.7488085518832,59.7464091592795,60.7440097666758,61.7416103740721,
62.7392109814685,63.7368115888648,64.7344121962611,65.7320128036574,66.7296134110537,
67.72721401845,68.7248146258463,69.7224152332426,70.7200158406389,71.7176164480352,
72.7152170554315,73.7128176628279,74.7104182702242,75.7080188776205,76.7056194850168,
77.7032200924131,78.7008206998094,79.6984213072057,80.696021914602,81.6936225219983,
82.6912231293946,83.688823736791,84.6864243441873,85.6840249515836),
 .UNSPECIFIED.);
#136=B_SPLINE_SURFACE_WITH_KNOTS('',3,3,((#15442,#15443,#15444,#15445,#15446,
#15447,#15448,#15449,#15450,#15451,#15452,#15453,#15454,#15455,#15456,#15457,
#15458,#15459,#15460,#15461,#15462,#15463,#15464,#15465,#15466,#15467,#15468,
#15469,#15470,#15471,#15472,#15473,#15474,#15475,#15476,#15477,#15478,#15479,
#15480,#15481,#15482,#15483,#15484,#15485,#15486,#15487,#15488,#15489,#15490,
#15491,#15492,#15493,#15494,#15495,#15496,#15497,#15498,#15499,#15500,#15501,
#15502,#15503,#15504,#15505,#15506,#15507,#15508,#15509,#15510,#15511,#15512,
#15513,#15514,#15515,#15516,#15517,#15518),(#15519,#15520,#15521,#15522,
#15523,#15524,#15525,#15526,#15527,#15528,#15529,#15530,#15531,#15532,#15533,
#15534,#15535,#15536,#15537,#15538,#15539,#15540,#15541,#15542,#15543,#15544,
#15545,#15546,#15547,#15548,#15549,#15550,#15551,#15552,#15553,#15554,#15555,
#15556,#15557,#15558,#15559,#15560,#15561,#15562,#15563,#15564,#15565,#15566,
#15567,#15568,#15569,#15570,#15571,#15572,#15573,#15574,#15575,#15576,#15577,
#15578,#15579,#15580,#15581,#15582,#15583,#15584,#15585,#15586,#15587,#15588,
#15589,#15590,#15591,#15592,#15593,#15594,#15595),(#15596,#15597,#15598,
#15599,#15600,#15601,#15602,#15603,#15604,#15605,#15606,#15607,#15608,#15609,
#15610,#15611,#15612,#15613,#15614,#15615,#15616,#15617,#15618,#15619,#15620,
#15621,#15622,#15623,#15624,#15625,#15626,#15627,#15628,#15629,#15630,#15631,
#15632,#15633,#15634,#15635,#15636,#15637,#15638,#15639,#15640,#15641,#15642,
#15643,#15644,#15645,#15646,#15647,#15648,#15649,#15650,#15651,#15652,#15653,
#15654,#15655,#15656,#15657,#15658,#15659,#15660,#15661,#15662,#15663,#15664,
#15665,#15666,#15667,#15668,#15669,#15670,#15671,#15672),(#15673,#15674,
#15675,#15676,#15677,#15678,#15679,#15680,#15681,#15682,#15683,#15684,#15685,
#15686,#15687,#15688,#15689,#15690,#15691,#15692,#15693,#15694,#15695,#15696,
#15697,#15698,#15699,#15700,#15701,#15702,#15703,#15704,#15705,#15706,#15707,
#15708,#15709,#15710,#15711,#15712,#15713,#15714,#15715,#15716,#15717,#15718,
#15719,#15720,#15721,#15722,#15723,#15724,#15725,#15726,#15727,#15728,#15729,
#15730,#15731,#15732,#15733,#15734,#15735,#15736,#15737,#15738,#15739,#15740,
#15741,#15742,#15743,#15744,#15745,#15746,#15747,#15748,#15749)),
 .UNSPECIFIED.,.F.,.F.,.F.,(4,4),(4,1,1,1,1,1,1,1,1,1,1,1,1,1,1,1,1,1,1,
1,1,1,1,1,1,1,1,1,1,1,1,1,1,1,1,1,1,1,1,1,1,1,1,1,1,1,1,1,1,1,1,1,1,1,1,
1,1,1,1,1,1,1,1,1,1,1,1,1,1,1,1,1,1,1,4),(0.,0.0448889834294934),(14.3981410127769,
15.3957416201732,16.3933422275696,17.3909428349659,18.3885434423622,19.3861440497585,
20.3837446571548,21.3813452645511,22.3789458719474,23.3765464793437,24.37414708674,
25.3717476941363,26.3693483015326,27.366948908929,28.3645495163253,29.3621501237216,
30.3597507311179,31.3573513385142,32.3549519459105,33.3525525533068,34.3501531607031,
35.3477537680994,36.3453543754957,37.342954982892,38.3405555902884,39.3381561976847,
40.335756805081,41.3333574124773,42.3309580198736,43.3285586272699,44.3261592346662,
45.3237598420625,46.3213604494588,47.3189610568551,48.3165616642514,49.3141622716478,
50.3117628790441,51.3093634864404,52.3069640938367,53.304564701233,54.3021653086293,
55.2997659160256,56.2973665234219,57.2949671308182,58.2925677382145,59.2901683456108,
60.2877689530072,61.2853695604035,62.2829701677998,63.2805707751961,64.2781713825924,
65.2757719899887,66.273372597385,67.2709732047813,68.2685738121776,69.2661744195739,
70.2637750269702,71.2613756343666,72.2589762417629,73.2565768491592,74.2541774565555,
75.2517780639518,76.2493786713481,77.2469792787444,78.2445798861407,79.242180493537,
80.2397811009333,81.2373817083296,82.2349823157259,83.2325829231223,84.2301835305186,
85.2277841379149,86.2253847453112,87.2229853527075,88.2205859601038),
 .UNSPECIFIED.);
#137=B_SPLINE_SURFACE_WITH_KNOTS('',3,3,((#17361,#17362,#17363,#17364,#17365,
#17366,#17367,#17368,#17369,#17370,#17371,#17372,#17373,#17374,#17375,#17376,
#17377,#17378,#17379,#17380,#17381,#17382,#17383,#17384,#17385,#17386,#17387,
#17388,#17389,#17390,#17391,#17392,#17393,#17394,#17395,#17396,#17397,#17398,
#17399,#17400,#17401,#17402,#17403,#17404,#17405,#17406,#17407,#17408,#17409,
#17410,#17411,#17412,#17413,#17414,#17415,#17416,#17417,#17418,#17419,#17420,
#17421,#17422,#17423,#17424,#17425,#17426,#17427,#17428,#17429,#17430),
(#17431,#17432,#17433,#17434,#17435,#17436,#17437,#17438,#17439,#17440,
#17441,#17442,#17443,#17444,#17445,#17446,#17447,#17448,#17449,#17450,#17451,
#17452,#17453,#17454,#17455,#17456,#17457,#17458,#17459,#17460,#17461,#17462,
#17463,#17464,#17465,#17466,#17467,#17468,#17469,#17470,#17471,#17472,#17473,
#17474,#17475,#17476,#17477,#17478,#17479,#17480,#17481,#17482,#17483,#17484,
#17485,#17486,#17487,#17488,#17489,#17490,#17491,#17492,#17493,#17494,#17495,
#17496,#17497,#17498,#17499,#17500),(#17501,#17502,#17503,#17504,#17505,
#17506,#17507,#17508,#17509,#17510,#17511,#17512,#17513,#17514,#17515,#17516,
#17517,#17518,#17519,#17520,#17521,#17522,#17523,#17524,#17525,#17526,#17527,
#17528,#17529,#17530,#17531,#17532,#17533,#17534,#17535,#17536,#17537,#17538,
#17539,#17540,#17541,#17542,#17543,#17544,#17545,#17546,#17547,#17548,#17549,
#17550,#17551,#17552,#17553,#17554,#17555,#17556,#17557,#17558,#17559,#17560,
#17561,#17562,#17563,#17564,#17565,#17566,#17567,#17568,#17569,#17570),
(#17571,#17572,#17573,#17574,#17575,#17576,#17577,#17578,#17579,#17580,
#17581,#17582,#17583,#17584,#17585,#17586,#17587,#17588,#17589,#17590,#17591,
#17592,#17593,#17594,#17595,#17596,#17597,#17598,#17599,#17600,#17601,#17602,
#17603,#17604,#17605,#17606,#17607,#17608,#17609,#17610,#17611,#17612,#17613,
#17614,#17615,#17616,#17617,#17618,#17619,#17620,#17621,#17622,#17623,#17624,
#17625,#17626,#17627,#17628,#17629,#17630,#17631,#17632,#17633,#17634,#17635,
#17636,#17637,#17638,#17639,#17640)),.UNSPECIFIED.,.F.,.F.,.F.,(4,4),(4,
1,1,1,1,1,1,1,1,1,1,1,1,1,1,1,1,1,1,1,1,1,1,1,1,1,1,1,1,1,1,1,1,1,1,1,1,
1,1,1,1,1,1,1,1,1,1,1,1,1,1,1,1,1,1,1,1,1,1,1,1,1,1,1,1,1,1,4),(0.,0.0460148164544132),
(11.6154215191106,12.6127599630189,13.6100984069272,14.6074368508354,15.6047752947437,
16.602113738652,17.5994521825603,18.5967906264686,19.5941290703769,20.5914675142851,
21.5888059581934,22.5861444021017,23.58348284601,24.5808212899183,25.5781597338266,
26.5754981777348,27.5728366216431,28.5701750655514,29.5675135094597,30.564851953368,
31.5621903972762,32.5595288411845,33.5568672850928,34.5542057290011,35.5515441729094,
36.5488826168177,37.5462210607259,38.5435595046342,39.5408979485425,40.5382363924508,
41.5355748363591,42.5329132802674,43.5302517241756,44.5275901680839,45.5249286119922,
46.5222670559005,47.5196054998088,48.516943943717,49.5142823876253,50.5116208315336,
51.5089592754419,52.5062977193502,53.5036361632585,54.5009746071667,55.498313051075,
56.4956514949833,57.4929899388916,58.4903283827999,59.4876668267081,60.4850052706164,
61.4823437145247,62.479682158433,63.4770206023413,64.4743590462496,65.4716974901578,
66.4690359340661,67.4663743779744,68.4637128218827,69.461051265791,70.4583897096992,
71.4557281536075,72.4530665975158,73.4504050414241,74.4477434853324,75.4450819292407,
76.4424203731489,77.4397588170572,78.4370972609655),.UNSPECIFIED.);
#138=B_SPLINE_SURFACE_WITH_KNOTS('',3,3,((#17766,#17767,#17768,#17769,#17770,
#17771,#17772,#17773,#17774,#17775,#17776,#17777,#17778,#17779,#17780,#17781,
#17782,#17783,#17784,#17785,#17786,#17787,#17788,#17789,#17790,#17791,#17792,
#17793,#17794,#17795,#17796,#17797,#17798,#17799,#17800,#17801,#17802,#17803,
#17804,#17805,#17806,#17807,#17808,#17809,#17810,#17811,#17812,#17813,#17814,
#17815,#17816,#17817,#17818,#17819,#17820,#17821,#17822,#17823,#17824,#17825,
#17826,#17827,#17828,#17829,#17830,#17831,#17832,#17833,#17834,#17835,#17836,
#17837),(#17838,#17839,#17840,#17841,#17842,#17843,#17844,#17845,#17846,
#17847,#17848,#17849,#17850,#17851,#17852,#17853,#17854,#17855,#17856,#17857,
#17858,#17859,#17860,#17861,#17862,#17863,#17864,#17865,#17866,#17867,#17868,
#17869,#17870,#17871,#17872,#17873,#17874,#17875,#17876,#17877,#17878,#17879,
#17880,#17881,#17882,#17883,#17884,#17885,#17886,#17887,#17888,#17889,#17890,
#17891,#17892,#17893,#17894,#17895,#17896,#17897,#17898,#17899,#17900,#17901,
#17902,#17903,#17904,#17905,#17906,#17907,#17908,#17909),(#17910,#17911,
#17912,#17913,#17914,#17915,#17916,#17917,#17918,#17919,#17920,#17921,#17922,
#17923,#17924,#17925,#17926,#17927,#17928,#17929,#17930,#17931,#17932,#17933,
#17934,#17935,#17936,#17937,#17938,#17939,#17940,#17941,#17942,#17943,#17944,
#17945,#17946,#17947,#17948,#17949,#17950,#17951,#17952,#17953,#17954,#17955,
#17956,#17957,#17958,#17959,#17960,#17961,#17962,#17963,#17964,#17965,#17966,
#17967,#17968,#17969,#17970,#17971,#17972,#17973,#17974,#17975,#17976,#17977,
#17978,#17979,#17980,#17981),(#17982,#17983,#17984,#17985,#17986,#17987,
#17988,#17989,#17990,#17991,#17992,#17993,#17994,#17995,#17996,#17997,#17998,
#17999,#18000,#18001,#18002,#18003,#18004,#18005,#18006,#18007,#18008,#18009,
#18010,#18011,#18012,#18013,#18014,#18015,#18016,#18017,#18018,#18019,#18020,
#18021,#18022,#18023,#18024,#18025,#18026,#18027,#18028,#18029,#18030,#18031,
#18032,#18033,#18034,#18035,#18036,#18037,#18038,#18039,#18040,#18041,#18042,
#18043,#18044,#18045,#18046,#18047,#18048,#18049,#18050,#18051,#18052,#18053)),
 .UNSPECIFIED.,.F.,.F.,.F.,(4,4),(4,1,1,1,1,1,1,1,1,1,1,1,1,1,1,1,1,1,1,
1,1,1,1,1,1,1,1,1,1,1,1,1,1,1,1,1,1,1,1,1,1,1,1,1,1,1,1,1,1,1,1,1,1,1,1,
1,1,1,1,1,1,1,1,1,1,1,1,1,1,4),(0.,0.0460148164544132),(8.31058692273974,
9.30894657310399,10.3073062234682,11.3056658738325,12.3040255241967,13.302385174561,
14.3007448249252,15.2991044752895,16.2974641256537,17.295823776018,18.2941834263822,
19.2925430767465,20.2909027271107,21.289262377475,22.2876220278392,23.2859816782034,
24.2843413285677,25.2827009789319,26.2810606292962,27.2794202796604,28.2777799300247,
29.2761395803889,30.2744992307532,31.2728588811174,32.2712185314817,33.2695781818459,
34.2679378322102,35.2662974825744,36.2646571329387,37.2630167833029,38.2613764336672,
39.2597360840314,40.2580957343957,41.2564553847599,42.2548150351241,43.2531746854884,
44.2515343358526,45.2498939862169,46.2482536365811,47.2466132869454,48.2449729373096,
49.2433325876739,50.2416922380381,51.2400518884024,52.2384115387666,53.2367711891309,
54.2351308394951,55.2334904898594,56.2318501402236,57.2302097905879,58.2285694409521,
59.2269290913164,60.2252887416806,61.2236483920448,62.2220080424091,63.2203676927733,
64.2187273431376,65.2170869935018,66.2154466438661,67.2138062942303,68.2121659445946,
69.2105255949588,70.2088852453231,71.2072448956873,72.2056045460516,73.2039641964158,
74.2023238467801,75.2006834971443,76.1990431475085,77.1974027978728),
 .UNSPECIFIED.);
#139=B_SPLINE_SURFACE_WITH_KNOTS('',3,3,((#19619,#19620,#19621,#19622,#19623,
#19624,#19625,#19626,#19627,#19628,#19629,#19630,#19631,#19632,#19633,#19634,
#19635,#19636,#19637,#19638,#19639,#19640,#19641,#19642,#19643,#19644,#19645,
#19646,#19647,#19648,#19649,#19650,#19651,#19652,#19653,#19654,#19655,#19656,
#19657,#19658,#19659,#19660,#19661,#19662,#19663,#19664,#19665,#19666,#19667,
#19668,#19669,#19670,#19671,#19672,#19673,#19674,#19675,#19676,#19677,#19678,
#19679,#19680,#19681,#19682,#19683,#19684,#19685,#19686,#19687,#19688,#19689,
#19690,#19691,#19692,#19693,#19694,#19695,#19696,#19697,#19698,#19699,#19700,
#19701,#19702,#19703,#19704,#19705,#19706,#19707,#19708,#19709,#19710,#19711,
#19712,#19713,#19714,#19715,#19716,#19717,#19718,#19719,#19720),(#19721,
#19722,#19723,#19724,#19725,#19726,#19727,#19728,#19729,#19730,#19731,#19732,
#19733,#19734,#19735,#19736,#19737,#19738,#19739,#19740,#19741,#19742,#19743,
#19744,#19745,#19746,#19747,#19748,#19749,#19750,#19751,#19752,#19753,#19754,
#19755,#19756,#19757,#19758,#19759,#19760,#19761,#19762,#19763,#19764,#19765,
#19766,#19767,#19768,#19769,#19770,#19771,#19772,#19773,#19774,#19775,#19776,
#19777,#19778,#19779,#19780,#19781,#19782,#19783,#19784,#19785,#19786,#19787,
#19788,#19789,#19790,#19791,#19792,#19793,#19794,#19795,#19796,#19797,#19798,
#19799,#19800,#19801,#19802,#19803,#19804,#19805,#19806,#19807,#19808,#19809,
#19810,#19811,#19812,#19813,#19814,#19815,#19816,#19817,#19818,#19819,#19820,
#19821,#19822),(#19823,#19824,#19825,#19826,#19827,#19828,#19829,#19830,
#19831,#19832,#19833,#19834,#19835,#19836,#19837,#19838,#19839,#19840,#19841,
#19842,#19843,#19844,#19845,#19846,#19847,#19848,#19849,#19850,#19851,#19852,
#19853,#19854,#19855,#19856,#19857,#19858,#19859,#19860,#19861,#19862,#19863,
#19864,#19865,#19866,#19867,#19868,#19869,#19870,#19871,#19872,#19873,#19874,
#19875,#19876,#19877,#19878,#19879,#19880,#19881,#19882,#19883,#19884,#19885,
#19886,#19887,#19888,#19889,#19890,#19891,#19892,#19893,#19894,#19895,#19896,
#19897,#19898,#19899,#19900,#19901,#19902,#19903,#19904,#19905,#19906,#19907,
#19908,#19909,#19910,#19911,#19912,#19913,#19914,#19915,#19916,#19917,#19918,
#19919,#19920,#19921,#19922,#19923,#19924),(#19925,#19926,#19927,#19928,
#19929,#19930,#19931,#19932,#19933,#19934,#19935,#19936,#19937,#19938,#19939,
#19940,#19941,#19942,#19943,#19944,#19945,#19946,#19947,#19948,#19949,#19950,
#19951,#19952,#19953,#19954,#19955,#19956,#19957,#19958,#19959,#19960,#19961,
#19962,#19963,#19964,#19965,#19966,#19967,#19968,#19969,#19970,#19971,#19972,
#19973,#19974,#19975,#19976,#19977,#19978,#19979,#19980,#19981,#19982,#19983,
#19984,#19985,#19986,#19987,#19988,#19989,#19990,#19991,#19992,#19993,#19994,
#19995,#19996,#19997,#19998,#19999,#20000,#20001,#20002,#20003,#20004,#20005,
#20006,#20007,#20008,#20009,#20010,#20011,#20012,#20013,#20014,#20015,#20016,
#20017,#20018,#20019,#20020,#20021,#20022,#20023,#20024,#20025,#20026)),
 .UNSPECIFIED.,.F.,.F.,.F.,(4,4),(4,1,1,1,1,1,1,1,1,1,1,1,1,1,1,1,1,1,1,
1,1,1,1,1,1,1,1,1,1,1,1,1,1,1,1,1,1,1,1,1,1,1,1,1,1,1,1,1,1,1,1,1,1,1,1,
1,1,1,1,1,1,1,1,1,1,1,1,1,1,1,1,1,1,1,1,1,1,1,1,1,1,1,1,1,1,1,1,1,1,1,1,
1,1,1,1,1,1,1,1,4),(0.,0.0658467982010768),(11.6150328478182,12.6069034617266,
13.598774075635,14.5906446895433,15.5825153034517,16.5743859173601,17.5662565312685,
18.5581271451769,19.5499977590852,20.5418683729936,21.533738986902,22.5256096008104,
23.5174802147187,24.5093508286271,25.5012214425355,26.4930920564439,27.4849626703523,
28.4768332842606,29.468703898169,30.4605745120774,31.4524451259858,32.4443157398941,
33.4361863538025,34.4280569677109,35.4199275816193,36.4117981955277,37.403668809436,
38.3955394233444,39.3874100372528,40.3792806511612,41.3711512650695,42.3630218789779,
43.3548924928863,44.3467631067947,45.3386337207031,46.3305043346114,47.3223749485198,
48.3142455624282,49.3061161763366,50.2979867902449,51.2898574041533,52.2817280180617,
53.2735986319701,54.2654692458785,55.2573398597868,56.2492104736952,57.2410810876036,
58.232951701512,59.2248223154203,60.2166929293287,61.2085635432371,62.2004341571455,
63.1923047710539,64.1841753849622,65.1760459988706,66.167916612779,67.1597872266874,
68.1516578405957,69.1435284545041,70.1353990684125,71.1272696823209,72.1191402962293,
73.1110109101376,74.102881524046,75.0947521379544,76.0866227518628,77.0784933657711,
78.0703639796795,79.0622345935879,80.0541052074963,81.0459758214047,82.037846435313,
83.0297170492214,84.0215876631298,85.0134582770382,86.0053288909465,86.9971995048549,
87.9890701187633,88.9809407326717,89.9728113465801,90.9646819604884,91.9565525743968,
92.9484231883052,93.9402938022136,94.9321644161219,95.9240350300303,96.9159056439387,
97.9077762578471,98.8996468717555,99.8915174856638,100.883388099572,101.875258713481,
102.867129327389,103.858999941297,104.850870555206,105.842741169114,106.834611783022,
107.826482396931,108.818353010839,109.810223624748),.UNSPECIFIED.);
#140=B_SPLINE_SURFACE_WITH_KNOTS('',3,3,((#20155,#20156,#20157,#20158,#20159,
#20160,#20161,#20162,#20163,#20164,#20165,#20166,#20167,#20168,#20169,#20170,
#20171,#20172,#20173,#20174,#20175,#20176,#20177,#20178,#20179,#20180,#20181,
#20182,#20183,#20184,#20185,#20186,#20187,#20188,#20189,#20190,#20191,#20192,
#20193,#20194,#20195,#20196,#20197,#20198,#20199,#20200,#20201,#20202,#20203,
#20204,#20205,#20206,#20207,#20208,#20209,#20210,#20211,#20212,#20213,#20214,
#20215,#20216,#20217,#20218,#20219,#20220,#20221,#20222,#20223,#20224,#20225,
#20226,#20227,#20228,#20229,#20230,#20231,#20232,#20233,#20234,#20235,#20236,
#20237,#20238,#20239,#20240,#20241,#20242,#20243,#20244,#20245,#20246,#20247,
#20248,#20249,#20250,#20251,#20252,#20253,#20254,#20255,#20256,#20257,#20258),
(#20259,#20260,#20261,#20262,#20263,#20264,#20265,#20266,#20267,#20268,
#20269,#20270,#20271,#20272,#20273,#20274,#20275,#20276,#20277,#20278,#20279,
#20280,#20281,#20282,#20283,#20284,#20285,#20286,#20287,#20288,#20289,#20290,
#20291,#20292,#20293,#20294,#20295,#20296,#20297,#20298,#20299,#20300,#20301,
#20302,#20303,#20304,#20305,#20306,#20307,#20308,#20309,#20310,#20311,#20312,
#20313,#20314,#20315,#20316,#20317,#20318,#20319,#20320,#20321,#20322,#20323,
#20324,#20325,#20326,#20327,#20328,#20329,#20330,#20331,#20332,#20333,#20334,
#20335,#20336,#20337,#20338,#20339,#20340,#20341,#20342,#20343,#20344,#20345,
#20346,#20347,#20348,#20349,#20350,#20351,#20352,#20353,#20354,#20355,#20356,
#20357,#20358,#20359,#20360,#20361,#20362),(#20363,#20364,#20365,#20366,
#20367,#20368,#20369,#20370,#20371,#20372,#20373,#20374,#20375,#20376,#20377,
#20378,#20379,#20380,#20381,#20382,#20383,#20384,#20385,#20386,#20387,#20388,
#20389,#20390,#20391,#20392,#20393,#20394,#20395,#20396,#20397,#20398,#20399,
#20400,#20401,#20402,#20403,#20404,#20405,#20406,#20407,#20408,#20409,#20410,
#20411,#20412,#20413,#20414,#20415,#20416,#20417,#20418,#20419,#20420,#20421,
#20422,#20423,#20424,#20425,#20426,#20427,#20428,#20429,#20430,#20431,#20432,
#20433,#20434,#20435,#20436,#20437,#20438,#20439,#20440,#20441,#20442,#20443,
#20444,#20445,#20446,#20447,#20448,#20449,#20450,#20451,#20452,#20453,#20454,
#20455,#20456,#20457,#20458,#20459,#20460,#20461,#20462,#20463,#20464,#20465,
#20466),(#20467,#20468,#20469,#20470,#20471,#20472,#20473,#20474,#20475,
#20476,#20477,#20478,#20479,#20480,#20481,#20482,#20483,#20484,#20485,#20486,
#20487,#20488,#20489,#20490,#20491,#20492,#20493,#20494,#20495,#20496,#20497,
#20498,#20499,#20500,#20501,#20502,#20503,#20504,#20505,#20506,#20507,#20508,
#20509,#20510,#20511,#20512,#20513,#20514,#20515,#20516,#20517,#20518,#20519,
#20520,#20521,#20522,#20523,#20524,#20525,#20526,#20527,#20528,#20529,#20530,
#20531,#20532,#20533,#20534,#20535,#20536,#20537,#20538,#20539,#20540,#20541,
#20542,#20543,#20544,#20545,#20546,#20547,#20548,#20549,#20550,#20551,#20552,
#20553,#20554,#20555,#20556,#20557,#20558,#20559,#20560,#20561,#20562,#20563,
#20564,#20565,#20566,#20567,#20568,#20569,#20570)),.UNSPECIFIED.,.F.,.F.,
 .F.,(4,4),(4,1,1,1,1,1,1,1,1,1,1,1,1,1,1,1,1,1,1,1,1,1,1,1,1,1,1,1,1,1,
1,1,1,1,1,1,1,1,1,1,1,1,1,1,1,1,1,1,1,1,1,1,1,1,1,1,1,1,1,1,1,1,1,1,1,1,
1,1,1,1,1,1,1,1,1,1,1,1,1,1,1,1,1,1,1,1,1,1,1,1,1,1,1,1,1,1,1,1,1,1,1,4),
(0.,0.0658467982010768),(8.30747755240101,9.30018873014199,10.292899907883,
11.2856110856239,12.2783222633649,13.2710334411059,14.2637446188469,15.2564557965878,
16.2491669743288,17.2418781520698,18.2345893298108,19.2273005075518,20.2200116852927,
21.2127228630337,22.2054340407747,23.1981452185157,24.1908563962566,25.1835675739976,
26.1762787517386,27.1689899294796,28.1617011072206,29.1544122849615,30.1471234627025,
31.1398346404435,32.1325458181845,33.1252569959254,34.1179681736664,35.1106793514074,
36.1033905291484,37.0961017068893,38.0888128846303,39.0815240623713,40.0742352401123,
41.0669464178533,42.0596575955942,43.0523687733352,44.0450799510762,45.0377911288172,
46.0305023065581,47.0232134842991,48.0159246620401,49.0086358397811,50.001347017522,
50.994058195263,51.986769373004,52.979480550745,53.972191728486,54.9649029062269,
55.9576140839679,56.9503252617089,57.9430364394499,58.9357476171908,59.9284587949318,
60.9211699726728,61.9138811504138,62.9065923281547,63.8993035058957,64.8920146836367,
65.8847258613777,66.8774370391187,67.8701482168596,68.8628593946006,69.8555705723416,
70.8482817500825,71.8409929278235,72.8337041055645,73.8264152833055,74.8191264610465,
75.8118376387874,76.8045488165284,77.7972599942694,78.7899711720104,79.7826823497514,
80.7753935274923,81.7681047052333,82.7608158829743,83.7535270607153,84.7462382384562,
85.7389494161972,86.7316605939382,87.7243717716792,88.7170829494201,89.7097941271611,
90.7025053049021,91.6952164826431,92.687927660384,93.680638838125,94.673350015866,
95.666061193607,96.658772371348,97.6514835490889,98.6441947268299,99.6369059045709,
100.629617082312,101.622328260053,102.615039437794,103.607750615535,104.600461793276,
105.593172971017,106.585884148758,107.578595326499,108.57130650424),
 .UNSPECIFIED.);
#141=B_SPLINE_SURFACE_WITH_KNOTS('',3,3,((#21091,#21092,#21093,#21094,#21095,
#21096,#21097,#21098,#21099,#21100,#21101,#21102,#21103,#21104,#21105,#21106,
#21107,#21108,#21109,#21110,#21111,#21112,#21113,#21114,#21115,#21116,#21117,
#21118,#21119,#21120,#21121,#21122,#21123,#21124,#21125,#21126,#21127),
(#21128,#21129,#21130,#21131,#21132,#21133,#21134,#21135,#21136,#21137,
#21138,#21139,#21140,#21141,#21142,#21143,#21144,#21145,#21146,#21147,#21148,
#21149,#21150,#21151,#21152,#21153,#21154,#21155,#21156,#21157,#21158,#21159,
#21160,#21161,#21162,#21163,#21164),(#21165,#21166,#21167,#21168,#21169,
#21170,#21171,#21172,#21173,#21174,#21175,#21176,#21177,#21178,#21179,#21180,
#21181,#21182,#21183,#21184,#21185,#21186,#21187,#21188,#21189,#21190,#21191,
#21192,#21193,#21194,#21195,#21196,#21197,#21198,#21199,#21200,#21201),
(#21202,#21203,#21204,#21205,#21206,#21207,#21208,#21209,#21210,#21211,
#21212,#21213,#21214,#21215,#21216,#21217,#21218,#21219,#21220,#21221,#21222,
#21223,#21224,#21225,#21226,#21227,#21228,#21229,#21230,#21231,#21232,#21233,
#21234,#21235,#21236,#21237,#21238)),.UNSPECIFIED.,.F.,.F.,.F.,(4,4),(4,
1,1,1,1,1,1,1,1,1,1,1,1,1,1,1,1,1,1,1,1,1,1,1,1,1,1,1,1,1,1,1,1,1,4),(0.,
0.0642013499338864),(11.8589888623078,12.8423086102174,13.825628358127,
14.8089481060366,15.7922678539462,16.7755876018558,17.7589073497654,18.742227097675,
19.7255468455846,20.7088665934942,21.6921863414038,22.6755060893134,23.658825837223,
24.6421455851326,25.6254653330422,26.6087850809518,27.5921048288614,28.575424576771,
29.5587443246806,30.5420640725902,31.5253838204998,32.5087035684094,33.492023316319,
34.4753430642286,35.4586628121382,36.4419825600478,37.4253023079574,38.408622055867,
39.3919418037766,40.3752615516862,41.3585812995958,42.3419010475054,43.325220795415,
44.3085405433246,45.2918602912342),.UNSPECIFIED.);
#142=B_SPLINE_SURFACE_WITH_KNOTS('',3,3,((#21446,#21447,#21448,#21449,#21450,
#21451,#21452,#21453,#21454,#21455,#21456,#21457,#21458,#21459,#21460,#21461,
#21462,#21463,#21464,#21465,#21466,#21467,#21468,#21469,#21470,#21471,#21472,
#21473,#21474,#21475,#21476,#21477,#21478,#21479,#21480,#21481,#21482),
(#21483,#21484,#21485,#21486,#21487,#21488,#21489,#21490,#21491,#21492,
#21493,#21494,#21495,#21496,#21497,#21498,#21499,#21500,#21501,#21502,#21503,
#21504,#21505,#21506,#21507,#21508,#21509,#21510,#21511,#21512,#21513,#21514,
#21515,#21516,#21517,#21518,#21519),(#21520,#21521,#21522,#21523,#21524,
#21525,#21526,#21527,#21528,#21529,#21530,#21531,#21532,#21533,#21534,#21535,
#21536,#21537,#21538,#21539,#21540,#21541,#21542,#21543,#21544,#21545,#21546,
#21547,#21548,#21549,#21550,#21551,#21552,#21553,#21554,#21555,#21556),
(#21557,#21558,#21559,#21560,#21561,#21562,#21563,#21564,#21565,#21566,
#21567,#21568,#21569,#21570,#21571,#21572,#21573,#21574,#21575,#21576,#21577,
#21578,#21579,#21580,#21581,#21582,#21583,#21584,#21585,#21586,#21587,#21588,
#21589,#21590,#21591,#21592,#21593)),.UNSPECIFIED.,.F.,.F.,.F.,(4,4),(4,
1,1,1,1,1,1,1,1,1,1,1,1,1,1,1,1,1,1,1,1,1,1,1,1,1,1,1,1,1,1,1,1,1,4),(0.,
0.0642013499338863),(14.3984001269719,15.3817198748815,16.3650396227911,
17.3483593707007,18.3316791186103,19.3149988665199,20.2983186144295,21.2816383623391,
22.2649581102487,23.2482778581583,24.2315976060679,25.2149173539775,26.1982371018871,
27.1815568497966,28.1648765977063,29.1481963456159,30.1315160935254,31.114835841435,
32.0981555893446,33.0814753372542,34.0647950851639,35.0481148330734,36.031434580983,
37.0147543288926,37.9980740768022,38.9813938247118,39.9647135726214,40.948033320531,
41.9313530684406,42.9146728163502,43.8979925642598,44.8813123121694,45.864632060079,
46.8479518079886,47.8312715558982),.UNSPECIFIED.);
#143=TOROIDAL_SURFACE('',#6643,5.5,2.);
#144=TOROIDAL_SURFACE('',#6647,5.5,2.);
#145=FACE_BOUND('',#771,.T.);
#146=FACE_BOUND('',#786,.T.);
#147=FACE_BOUND('',#787,.T.);
#148=FACE_BOUND('',#788,.T.);
#149=FACE_BOUND('',#789,.T.);
#150=FACE_BOUND('',#790,.T.);
#151=FACE_BOUND('',#791,.T.);
#152=FACE_BOUND('',#792,.T.);
#153=FACE_BOUND('',#803,.T.);
#154=FACE_BOUND('',#804,.T.);
#155=FACE_BOUND('',#805,.T.);
#156=FACE_BOUND('',#827,.T.);
#157=FACE_BOUND('',#828,.T.);
#158=FACE_BOUND('',#829,.T.);
#159=FACE_BOUND('',#863,.T.);
#160=FACE_BOUND('',#864,.T.);
#161=FACE_BOUND('',#865,.T.);
#162=FACE_BOUND('',#869,.T.);
#163=FACE_BOUND('',#870,.T.);
#164=FACE_BOUND('',#871,.T.);
#165=FACE_BOUND('',#890,.T.);
#166=FACE_BOUND('',#891,.T.);
#167=FACE_BOUND('',#892,.T.);
#168=FACE_BOUND('',#894,.T.);
#169=FACE_BOUND('',#895,.T.);
#170=FACE_BOUND('',#896,.T.);
#171=FACE_BOUND('',#918,.T.);
#172=FACE_BOUND('',#919,.T.);
#173=FACE_BOUND('',#920,.T.);
#174=FACE_BOUND('',#921,.T.);
#175=FACE_BOUND('',#922,.T.);
#176=FACE_BOUND('',#923,.T.);
#177=FACE_BOUND('',#924,.T.);
#178=FACE_BOUND('',#926,.T.);
#179=FACE_BOUND('',#927,.T.);
#180=FACE_BOUND('',#928,.T.);
#181=FACE_BOUND('',#929,.T.);
#182=FACE_BOUND('',#930,.T.);
#183=FACE_BOUND('',#931,.T.);
#184=FACE_BOUND('',#932,.T.);
#185=FACE_BOUND('',#935,.T.);
#186=FACE_BOUND('',#938,.T.);
#187=FACE_BOUND('',#944,.T.);
#188=FACE_BOUND('',#947,.T.);
#189=FACE_BOUND('',#984,.T.);
#190=FACE_BOUND('',#987,.T.);
#191=FACE_BOUND('',#1032,.T.);
#192=FACE_BOUND('',#1035,.T.);
#193=FACE_BOUND('',#1040,.T.);
#194=FACE_BOUND('',#1042,.T.);
#195=FACE_BOUND('',#1057,.T.);
#196=FACE_BOUND('',#1066,.T.);
#197=PLANE('',#6626);
#198=PLANE('',#6627);
#199=PLANE('',#6628);
#200=PLANE('',#6629);
#201=PLANE('',#6641);
#202=PLANE('',#6642);
#203=PLANE('',#6656);
#204=PLANE('',#6660);
#205=PLANE('',#6661);
#206=PLANE('',#6663);
#207=PLANE('',#6666);
#208=PLANE('',#6668);
#209=PLANE('',#6669);
#210=PLANE('',#6670);
#211=PLANE('',#6671);
#212=PLANE('',#6672);
#213=PLANE('',#6673);
#214=PLANE('',#6674);
#215=PLANE('',#6675);
#216=PLANE('',#6676);
#217=PLANE('',#6677);
#218=PLANE('',#6678);
#219=PLANE('',#6679);
#220=PLANE('',#6680);
#221=PLANE('',#6681);
#222=PLANE('',#6682);
#223=PLANE('',#6683);
#224=PLANE('',#6684);
#225=PLANE('',#6685);
#226=PLANE('',#6686);
#227=PLANE('',#6687);
#228=PLANE('',#6688);
#229=PLANE('',#6689);
#230=PLANE('',#6690);
#231=PLANE('',#6691);
#232=PLANE('',#6692);
#233=PLANE('',#6738);
#234=PLANE('',#6739);
#235=PLANE('',#6742);
#236=PLANE('',#6743);
#237=PLANE('',#6744);
#238=PLANE('',#6747);
#239=PLANE('',#6750);
#240=PLANE('',#6751);
#241=PLANE('',#6752);
#242=PLANE('',#6753);
#243=PLANE('',#6761);
#244=PLANE('',#6762);
#245=PLANE('',#6763);
#246=PLANE('',#6764);
#247=PLANE('',#6765);
#248=PLANE('',#6766);
#249=PLANE('',#6767);
#250=PLANE('',#6768);
#251=PLANE('',#6769);
#252=PLANE('',#6770);
#253=PLANE('',#6784);
#254=PLANE('',#6785);
#255=PLANE('',#6786);
#256=PLANE('',#6787);
#257=PLANE('',#6788);
#258=PLANE('',#6789);
#259=PLANE('',#6790);
#260=PLANE('',#6791);
#261=PLANE('',#6792);
#262=PLANE('',#6793);
#263=PLANE('',#6794);
#264=PLANE('',#6795);
#265=PLANE('',#6796);
#266=PLANE('',#6797);
#267=PLANE('',#6798);
#268=PLANE('',#6799);
#269=PLANE('',#6800);
#270=PLANE('',#6801);
#271=PLANE('',#6806);
#272=PLANE('',#6807);
#273=PLANE('',#6808);
#274=PLANE('',#6809);
#275=PLANE('',#6810);
#276=PLANE('',#6811);
#277=PLANE('',#6816);
#278=PLANE('',#6817);
#279=PLANE('',#6818);
#280=PLANE('',#6819);
#281=PLANE('',#6820);
#282=PLANE('',#6821);
#283=PLANE('',#6851);
#284=PLANE('',#6852);
#285=PLANE('',#6853);
#286=PLANE('',#6854);
#287=PLANE('',#6855);
#288=PLANE('',#6856);
#289=PLANE('',#6857);
#290=PLANE('',#6858);
#291=PLANE('',#6862);
#292=PLANE('',#6863);
#293=PLANE('',#6903);
#294=PLANE('',#6904);
#295=PLANE('',#6905);
#296=PLANE('',#6906);
#297=PLANE('',#6907);
#298=PLANE('',#6908);
#299=PLANE('',#6909);
#300=PLANE('',#6910);
#301=PLANE('',#6914);
#302=PLANE('',#6915);
#303=PLANE('',#6923);
#304=PLANE('',#6924);
#305=PLANE('',#6941);
#306=PLANE('',#6943);
#307=PLANE('',#6944);
#308=PLANE('',#6945);
#309=PLANE('',#6946);
#310=PLANE('',#6947);
#311=PLANE('',#6948);
#312=PLANE('',#6949);
#313=ELLIPSE('',#6615,2.16478440058479,2.);
#314=ELLIPSE('',#6616,2.16478440058479,2.);
#315=ELLIPSE('',#6618,2.16478440058479,2.);
#316=ELLIPSE('',#6620,2.16478440058479,2.);
#317=ELLIPSE('',#6622,2.82842712474619,2.);
#318=ELLIPSE('',#6624,2.82842712474619,2.);
#319=ELLIPSE('',#6634,2.82842712474619,2.);
#320=ELLIPSE('',#6635,2.82842712474619,2.);
#321=ELLIPSE('',#6637,2.82842712474619,2.);
#322=ELLIPSE('',#6639,2.82842712474619,2.);
#323=FACE_OUTER_BOUND('',#669,.T.);
#324=FACE_OUTER_BOUND('',#670,.T.);
#325=FACE_OUTER_BOUND('',#671,.T.);
#326=FACE_OUTER_BOUND('',#672,.T.);
#327=FACE_OUTER_BOUND('',#673,.T.);
#328=FACE_OUTER_BOUND('',#674,.T.);
#329=FACE_OUTER_BOUND('',#675,.T.);
#330=FACE_OUTER_BOUND('',#676,.T.);
#331=FACE_OUTER_BOUND('',#677,.T.);
#332=FACE_OUTER_BOUND('',#678,.T.);
#333=FACE_OUTER_BOUND('',#679,.T.);
#334=FACE_OUTER_BOUND('',#680,.T.);
#335=FACE_OUTER_BOUND('',#681,.T.);
#336=FACE_OUTER_BOUND('',#682,.T.);
#337=FACE_OUTER_BOUND('',#683,.T.);
#338=FACE_OUTER_BOUND('',#684,.T.);
#339=FACE_OUTER_BOUND('',#685,.T.);
#340=FACE_OUTER_BOUND('',#686,.T.);
#341=FACE_OUTER_BOUND('',#687,.T.);
#342=FACE_OUTER_BOUND('',#688,.T.);
#343=FACE_OUTER_BOUND('',#689,.T.);
#344=FACE_OUTER_BOUND('',#690,.T.);
#345=FACE_OUTER_BOUND('',#691,.T.);
#346=FACE_OUTER_BOUND('',#692,.T.);
#347=FACE_OUTER_BOUND('',#693,.T.);
#348=FACE_OUTER_BOUND('',#694,.T.);
#349=FACE_OUTER_BOUND('',#695,.T.);
#350=FACE_OUTER_BOUND('',#696,.T.);
#351=FACE_OUTER_BOUND('',#697,.T.);
#352=FACE_OUTER_BOUND('',#698,.T.);
#353=FACE_OUTER_BOUND('',#699,.T.);
#354=FACE_OUTER_BOUND('',#700,.T.);
#355=FACE_OUTER_BOUND('',#701,.T.);
#356=FACE_OUTER_BOUND('',#702,.T.);
#357=FACE_OUTER_BOUND('',#703,.T.);
#358=FACE_OUTER_BOUND('',#704,.T.);
#359=FACE_OUTER_BOUND('',#705,.T.);
#360=FACE_OUTER_BOUND('',#706,.T.);
#361=FACE_OUTER_BOUND('',#707,.T.);
#362=FACE_OUTER_BOUND('',#708,.T.);
#363=FACE_OUTER_BOUND('',#709,.T.);
#364=FACE_OUTER_BOUND('',#710,.T.);
#365=FACE_OUTER_BOUND('',#711,.T.);
#366=FACE_OUTER_BOUND('',#712,.T.);
#367=FACE_OUTER_BOUND('',#713,.T.);
#368=FACE_OUTER_BOUND('',#714,.T.);
#369=FACE_OUTER_BOUND('',#715,.T.);
#370=FACE_OUTER_BOUND('',#716,.T.);
#371=FACE_OUTER_BOUND('',#717,.T.);
#372=FACE_OUTER_BOUND('',#718,.T.);
#373=FACE_OUTER_BOUND('',#719,.T.);
#374=FACE_OUTER_BOUND('',#720,.T.);
#375=FACE_OUTER_BOUND('',#721,.T.);
#376=FACE_OUTER_BOUND('',#722,.T.);
#377=FACE_OUTER_BOUND('',#723,.T.);
#378=FACE_OUTER_BOUND('',#724,.T.);
#379=FACE_OUTER_BOUND('',#725,.T.);
#380=FACE_OUTER_BOUND('',#726,.T.);
#381=FACE_OUTER_BOUND('',#727,.T.);
#382=FACE_OUTER_BOUND('',#728,.T.);
#383=FACE_OUTER_BOUND('',#729,.T.);
#384=FACE_OUTER_BOUND('',#730,.T.);
#385=FACE_OUTER_BOUND('',#731,.T.);
#386=FACE_OUTER_BOUND('',#732,.T.);
#387=FACE_OUTER_BOUND('',#733,.T.);
#388=FACE_OUTER_BOUND('',#734,.T.);
#389=FACE_OUTER_BOUND('',#735,.T.);
#390=FACE_OUTER_BOUND('',#736,.T.);
#391=FACE_OUTER_BOUND('',#737,.T.);
#392=FACE_OUTER_BOUND('',#738,.T.);
#393=FACE_OUTER_BOUND('',#739,.T.);
#394=FACE_OUTER_BOUND('',#740,.T.);
#395=FACE_OUTER_BOUND('',#741,.T.);
#396=FACE_OUTER_BOUND('',#742,.T.);
#397=FACE_OUTER_BOUND('',#743,.T.);
#398=FACE_OUTER_BOUND('',#744,.T.);
#399=FACE_OUTER_BOUND('',#745,.T.);
#400=FACE_OUTER_BOUND('',#746,.T.);
#401=FACE_OUTER_BOUND('',#747,.T.);
#402=FACE_OUTER_BOUND('',#748,.T.);
#403=FACE_OUTER_BOUND('',#749,.T.);
#404=FACE_OUTER_BOUND('',#750,.T.);
#405=FACE_OUTER_BOUND('',#751,.T.);
#406=FACE_OUTER_BOUND('',#752,.T.);
#407=FACE_OUTER_BOUND('',#753,.T.);
#408=FACE_OUTER_BOUND('',#754,.T.);
#409=FACE_OUTER_BOUND('',#755,.T.);
#410=FACE_OUTER_BOUND('',#756,.T.);
#411=FACE_OUTER_BOUND('',#757,.T.);
#412=FACE_OUTER_BOUND('',#758,.T.);
#413=FACE_OUTER_BOUND('',#759,.T.);
#414=FACE_OUTER_BOUND('',#760,.T.);
#415=FACE_OUTER_BOUND('',#761,.T.);
#416=FACE_OUTER_BOUND('',#762,.T.);
#417=FACE_OUTER_BOUND('',#763,.T.);
#418=FACE_OUTER_BOUND('',#764,.T.);
#419=FACE_OUTER_BOUND('',#765,.T.);
#420=FACE_OUTER_BOUND('',#766,.T.);
#421=FACE_OUTER_BOUND('',#767,.T.);
#422=FACE_OUTER_BOUND('',#768,.T.);
#423=FACE_OUTER_BOUND('',#769,.T.);
#424=FACE_OUTER_BOUND('',#770,.T.);
#425=FACE_OUTER_BOUND('',#772,.T.);
#426=FACE_OUTER_BOUND('',#773,.T.);
#427=FACE_OUTER_BOUND('',#774,.T.);
#428=FACE_OUTER_BOUND('',#775,.T.);
#429=FACE_OUTER_BOUND('',#776,.T.);
#430=FACE_OUTER_BOUND('',#777,.T.);
#431=FACE_OUTER_BOUND('',#778,.T.);
#432=FACE_OUTER_BOUND('',#779,.T.);
#433=FACE_OUTER_BOUND('',#780,.T.);
#434=FACE_OUTER_BOUND('',#781,.T.);
#435=FACE_OUTER_BOUND('',#782,.T.);
#436=FACE_OUTER_BOUND('',#783,.T.);
#437=FACE_OUTER_BOUND('',#784,.T.);
#438=FACE_OUTER_BOUND('',#785,.T.);
#439=FACE_OUTER_BOUND('',#793,.T.);
#440=FACE_OUTER_BOUND('',#794,.T.);
#441=FACE_OUTER_BOUND('',#795,.T.);
#442=FACE_OUTER_BOUND('',#796,.T.);
#443=FACE_OUTER_BOUND('',#797,.T.);
#444=FACE_OUTER_BOUND('',#798,.T.);
#445=FACE_OUTER_BOUND('',#799,.T.);
#446=FACE_OUTER_BOUND('',#800,.T.);
#447=FACE_OUTER_BOUND('',#801,.T.);
#448=FACE_OUTER_BOUND('',#802,.T.);
#449=FACE_OUTER_BOUND('',#806,.T.);
#450=FACE_OUTER_BOUND('',#807,.T.);
#451=FACE_OUTER_BOUND('',#808,.T.);
#452=FACE_OUTER_BOUND('',#809,.T.);
#453=FACE_OUTER_BOUND('',#810,.T.);
#454=FACE_OUTER_BOUND('',#811,.T.);
#455=FACE_OUTER_BOUND('',#812,.T.);
#456=FACE_OUTER_BOUND('',#813,.T.);
#457=FACE_OUTER_BOUND('',#814,.T.);
#458=FACE_OUTER_BOUND('',#815,.T.);
#459=FACE_OUTER_BOUND('',#816,.T.);
#460=FACE_OUTER_BOUND('',#817,.T.);
#461=FACE_OUTER_BOUND('',#818,.T.);
#462=FACE_OUTER_BOUND('',#819,.T.);
#463=FACE_OUTER_BOUND('',#820,.T.);
#464=FACE_OUTER_BOUND('',#821,.T.);
#465=FACE_OUTER_BOUND('',#822,.T.);
#466=FACE_OUTER_BOUND('',#823,.T.);
#467=FACE_OUTER_BOUND('',#824,.T.);
#468=FACE_OUTER_BOUND('',#825,.T.);
#469=FACE_OUTER_BOUND('',#826,.T.);
#470=FACE_OUTER_BOUND('',#830,.T.);
#471=FACE_OUTER_BOUND('',#831,.T.);
#472=FACE_OUTER_BOUND('',#832,.T.);
#473=FACE_OUTER_BOUND('',#833,.T.);
#474=FACE_OUTER_BOUND('',#834,.T.);
#475=FACE_OUTER_BOUND('',#835,.T.);
#476=FACE_OUTER_BOUND('',#836,.T.);
#477=FACE_OUTER_BOUND('',#837,.T.);
#478=FACE_OUTER_BOUND('',#838,.T.);
#479=FACE_OUTER_BOUND('',#839,.T.);
#480=FACE_OUTER_BOUND('',#840,.T.);
#481=FACE_OUTER_BOUND('',#841,.T.);
#482=FACE_OUTER_BOUND('',#842,.T.);
#483=FACE_OUTER_BOUND('',#843,.T.);
#484=FACE_OUTER_BOUND('',#844,.T.);
#485=FACE_OUTER_BOUND('',#845,.T.);
#486=FACE_OUTER_BOUND('',#846,.T.);
#487=FACE_OUTER_BOUND('',#847,.T.);
#488=FACE_OUTER_BOUND('',#848,.T.);
#489=FACE_OUTER_BOUND('',#849,.T.);
#490=FACE_OUTER_BOUND('',#850,.T.);
#491=FACE_OUTER_BOUND('',#851,.T.);
#492=FACE_OUTER_BOUND('',#852,.T.);
#493=FACE_OUTER_BOUND('',#853,.T.);
#494=FACE_OUTER_BOUND('',#854,.T.);
#495=FACE_OUTER_BOUND('',#855,.T.);
#496=FACE_OUTER_BOUND('',#856,.T.);
#497=FACE_OUTER_BOUND('',#857,.T.);
#498=FACE_OUTER_BOUND('',#858,.T.);
#499=FACE_OUTER_BOUND('',#859,.T.);
#500=FACE_OUTER_BOUND('',#860,.T.);
#501=FACE_OUTER_BOUND('',#861,.T.);
#502=FACE_OUTER_BOUND('',#862,.T.);
#503=FACE_OUTER_BOUND('',#866,.T.);
#504=FACE_OUTER_BOUND('',#867,.T.);
#505=FACE_OUTER_BOUND('',#868,.T.);
#506=FACE_OUTER_BOUND('',#872,.T.);
#507=FACE_OUTER_BOUND('',#873,.T.);
#508=FACE_OUTER_BOUND('',#874,.T.);
#509=FACE_OUTER_BOUND('',#875,.T.);
#510=FACE_OUTER_BOUND('',#876,.T.);
#511=FACE_OUTER_BOUND('',#877,.T.);
#512=FACE_OUTER_BOUND('',#878,.T.);
#513=FACE_OUTER_BOUND('',#879,.T.);
#514=FACE_OUTER_BOUND('',#880,.T.);
#515=FACE_OUTER_BOUND('',#881,.T.);
#516=FACE_OUTER_BOUND('',#882,.T.);
#517=FACE_OUTER_BOUND('',#883,.T.);
#518=FACE_OUTER_BOUND('',#884,.T.);
#519=FACE_OUTER_BOUND('',#885,.T.);
#520=FACE_OUTER_BOUND('',#886,.T.);
#521=FACE_OUTER_BOUND('',#887,.T.);
#522=FACE_OUTER_BOUND('',#888,.T.);
#523=FACE_OUTER_BOUND('',#889,.T.);
#524=FACE_OUTER_BOUND('',#893,.T.);
#525=FACE_OUTER_BOUND('',#897,.T.);
#526=FACE_OUTER_BOUND('',#898,.T.);
#527=FACE_OUTER_BOUND('',#899,.T.);
#528=FACE_OUTER_BOUND('',#900,.T.);
#529=FACE_OUTER_BOUND('',#901,.T.);
#530=FACE_OUTER_BOUND('',#902,.T.);
#531=FACE_OUTER_BOUND('',#903,.T.);
#532=FACE_OUTER_BOUND('',#904,.T.);
#533=FACE_OUTER_BOUND('',#905,.T.);
#534=FACE_OUTER_BOUND('',#906,.T.);
#535=FACE_OUTER_BOUND('',#907,.T.);
#536=FACE_OUTER_BOUND('',#908,.T.);
#537=FACE_OUTER_BOUND('',#909,.T.);
#538=FACE_OUTER_BOUND('',#910,.T.);
#539=FACE_OUTER_BOUND('',#911,.T.);
#540=FACE_OUTER_BOUND('',#912,.T.);
#541=FACE_OUTER_BOUND('',#913,.T.);
#542=FACE_OUTER_BOUND('',#914,.T.);
#543=FACE_OUTER_BOUND('',#915,.T.);
#544=FACE_OUTER_BOUND('',#916,.T.);
#545=FACE_OUTER_BOUND('',#917,.T.);
#546=FACE_OUTER_BOUND('',#925,.T.);
#547=FACE_OUTER_BOUND('',#933,.T.);
#548=FACE_OUTER_BOUND('',#934,.T.);
#549=FACE_OUTER_BOUND('',#936,.T.);
#550=FACE_OUTER_BOUND('',#937,.T.);
#551=FACE_OUTER_BOUND('',#939,.T.);
#552=FACE_OUTER_BOUND('',#940,.T.);
#553=FACE_OUTER_BOUND('',#941,.T.);
#554=FACE_OUTER_BOUND('',#942,.T.);
#555=FACE_OUTER_BOUND('',#943,.T.);
#556=FACE_OUTER_BOUND('',#945,.T.);
#557=FACE_OUTER_BOUND('',#946,.T.);
#558=FACE_OUTER_BOUND('',#948,.T.);
#559=FACE_OUTER_BOUND('',#949,.T.);
#560=FACE_OUTER_BOUND('',#950,.T.);
#561=FACE_OUTER_BOUND('',#951,.T.);
#562=FACE_OUTER_BOUND('',#952,.T.);
#563=FACE_OUTER_BOUND('',#953,.T.);
#564=FACE_OUTER_BOUND('',#954,.T.);
#565=FACE_OUTER_BOUND('',#955,.T.);
#566=FACE_OUTER_BOUND('',#956,.T.);
#567=FACE_OUTER_BOUND('',#957,.T.);
#568=FACE_OUTER_BOUND('',#958,.T.);
#569=FACE_OUTER_BOUND('',#959,.T.);
#570=FACE_OUTER_BOUND('',#960,.T.);
#571=FACE_OUTER_BOUND('',#961,.T.);
#572=FACE_OUTER_BOUND('',#962,.T.);
#573=FACE_OUTER_BOUND('',#963,.T.);
#574=FACE_OUTER_BOUND('',#964,.T.);
#575=FACE_OUTER_BOUND('',#965,.T.);
#576=FACE_OUTER_BOUND('',#966,.T.);
#577=FACE_OUTER_BOUND('',#967,.T.);
#578=FACE_OUTER_BOUND('',#968,.T.);
#579=FACE_OUTER_BOUND('',#969,.T.);
#580=FACE_OUTER_BOUND('',#970,.T.);
#581=FACE_OUTER_BOUND('',#971,.T.);
#582=FACE_OUTER_BOUND('',#972,.T.);
#583=FACE_OUTER_BOUND('',#973,.T.);
#584=FACE_OUTER_BOUND('',#974,.T.);
#585=FACE_OUTER_BOUND('',#975,.T.);
#586=FACE_OUTER_BOUND('',#976,.T.);
#587=FACE_OUTER_BOUND('',#977,.T.);
#588=FACE_OUTER_BOUND('',#978,.T.);
#589=FACE_OUTER_BOUND('',#979,.T.);
#590=FACE_OUTER_BOUND('',#980,.T.);
#591=FACE_OUTER_BOUND('',#981,.T.);
#592=FACE_OUTER_BOUND('',#982,.T.);
#593=FACE_OUTER_BOUND('',#983,.T.);
#594=FACE_OUTER_BOUND('',#985,.T.);
#595=FACE_OUTER_BOUND('',#986,.T.);
#596=FACE_OUTER_BOUND('',#988,.T.);
#597=FACE_OUTER_BOUND('',#989,.T.);
#598=FACE_OUTER_BOUND('',#990,.T.);
#599=FACE_OUTER_BOUND('',#991,.T.);
#600=FACE_OUTER_BOUND('',#992,.T.);
#601=FACE_OUTER_BOUND('',#993,.T.);
#602=FACE_OUTER_BOUND('',#994,.T.);
#603=FACE_OUTER_BOUND('',#995,.T.);
#604=FACE_OUTER_BOUND('',#996,.T.);
#605=FACE_OUTER_BOUND('',#997,.T.);
#606=FACE_OUTER_BOUND('',#998,.T.);
#607=FACE_OUTER_BOUND('',#999,.T.);
#608=FACE_OUTER_BOUND('',#1000,.T.);
#609=FACE_OUTER_BOUND('',#1001,.T.);
#610=FACE_OUTER_BOUND('',#1002,.T.);
#611=FACE_OUTER_BOUND('',#1003,.T.);
#612=FACE_OUTER_BOUND('',#1004,.T.);
#613=FACE_OUTER_BOUND('',#1005,.T.);
#614=FACE_OUTER_BOUND('',#1006,.T.);
#615=FACE_OUTER_BOUND('',#1007,.T.);
#616=FACE_OUTER_BOUND('',#1008,.T.);
#617=FACE_OUTER_BOUND('',#1009,.T.);
#618=FACE_OUTER_BOUND('',#1010,.T.);
#619=FACE_OUTER_BOUND('',#1011,.T.);
#620=FACE_OUTER_BOUND('',#1012,.T.);
#621=FACE_OUTER_BOUND('',#1013,.T.);
#622=FACE_OUTER_BOUND('',#1014,.T.);
#623=FACE_OUTER_BOUND('',#1015,.T.);
#624=FACE_OUTER_BOUND('',#1016,.T.);
#625=FACE_OUTER_BOUND('',#1017,.T.);
#626=FACE_OUTER_BOUND('',#1018,.T.);
#627=FACE_OUTER_BOUND('',#1019,.T.);
#628=FACE_OUTER_BOUND('',#1020,.T.);
#629=FACE_OUTER_BOUND('',#1021,.T.);
#630=FACE_OUTER_BOUND('',#1022,.T.);
#631=FACE_OUTER_BOUND('',#1023,.T.);
#632=FACE_OUTER_BOUND('',#1024,.T.);
#633=FACE_OUTER_BOUND('',#1025,.T.);
#634=FACE_OUTER_BOUND('',#1026,.T.);
#635=FACE_OUTER_BOUND('',#1027,.T.);
#636=FACE_OUTER_BOUND('',#1028,.T.);
#637=FACE_OUTER_BOUND('',#1029,.T.);
#638=FACE_OUTER_BOUND('',#1030,.T.);
#639=FACE_OUTER_BOUND('',#1031,.T.);
#640=FACE_OUTER_BOUND('',#1033,.T.);
#641=FACE_OUTER_BOUND('',#1034,.T.);
#642=FACE_OUTER_BOUND('',#1036,.T.);
#643=FACE_OUTER_BOUND('',#1037,.T.);
#644=FACE_OUTER_BOUND('',#1038,.T.);
#645=FACE_OUTER_BOUND('',#1039,.T.);
#646=FACE_OUTER_BOUND('',#1041,.T.);
#647=FACE_OUTER_BOUND('',#1043,.T.);
#648=FACE_OUTER_BOUND('',#1044,.T.);
#649=FACE_OUTER_BOUND('',#1045,.T.);
#650=FACE_OUTER_BOUND('',#1046,.T.);
#651=FACE_OUTER_BOUND('',#1047,.T.);
#652=FACE_OUTER_BOUND('',#1048,.T.);
#653=FACE_OUTER_BOUND('',#1049,.T.);
#654=FACE_OUTER_BOUND('',#1050,.T.);
#655=FACE_OUTER_BOUND('',#1051,.T.);
#656=FACE_OUTER_BOUND('',#1052,.T.);
#657=FACE_OUTER_BOUND('',#1053,.T.);
#658=FACE_OUTER_BOUND('',#1054,.T.);
#659=FACE_OUTER_BOUND('',#1055,.T.);
#660=FACE_OUTER_BOUND('',#1056,.T.);
#661=FACE_OUTER_BOUND('',#1058,.T.);
#662=FACE_OUTER_BOUND('',#1059,.T.);
#663=FACE_OUTER_BOUND('',#1060,.T.);
#664=FACE_OUTER_BOUND('',#1061,.T.);
#665=FACE_OUTER_BOUND('',#1062,.T.);
#666=FACE_OUTER_BOUND('',#1063,.T.);
#667=FACE_OUTER_BOUND('',#1064,.T.);
#668=FACE_OUTER_BOUND('',#1065,.T.);
#669=EDGE_LOOP('',(#3975,#3976,#3977,#3978));
#670=EDGE_LOOP('',(#3979,#3980,#3981,#3982));
#671=EDGE_LOOP('',(#3983,#3984,#3985,#3986));
#672=EDGE_LOOP('',(#3987,#3988,#3989,#3990));
#673=EDGE_LOOP('',(#3991,#3992,#3993,#3994));
#674=EDGE_LOOP('',(#3995,#3996,#3997,#3998));
#675=EDGE_LOOP('',(#3999,#4000,#4001,#4002));
#676=EDGE_LOOP('',(#4003,#4004,#4005,#4006));
#677=EDGE_LOOP('',(#4007,#4008,#4009,#4010));
#678=EDGE_LOOP('',(#4011,#4012,#4013,#4014));
#679=EDGE_LOOP('',(#4015,#4016,#4017,#4018));
#680=EDGE_LOOP('',(#4019,#4020,#4021,#4022));
#681=EDGE_LOOP('',(#4023,#4024,#4025,#4026));
#682=EDGE_LOOP('',(#4027,#4028,#4029,#4030));
#683=EDGE_LOOP('',(#4031,#4032,#4033,#4034));
#684=EDGE_LOOP('',(#4035,#4036,#4037,#4038));
#685=EDGE_LOOP('',(#4039,#4040,#4041,#4042));
#686=EDGE_LOOP('',(#4043,#4044,#4045,#4046));
#687=EDGE_LOOP('',(#4047,#4048,#4049,#4050));
#688=EDGE_LOOP('',(#4051,#4052,#4053,#4054));
#689=EDGE_LOOP('',(#4055,#4056,#4057,#4058));
#690=EDGE_LOOP('',(#4059,#4060,#4061,#4062));
#691=EDGE_LOOP('',(#4063,#4064,#4065,#4066));
#692=EDGE_LOOP('',(#4067,#4068,#4069,#4070));
#693=EDGE_LOOP('',(#4071,#4072,#4073,#4074));
#694=EDGE_LOOP('',(#4075,#4076,#4077,#4078));
#695=EDGE_LOOP('',(#4079,#4080,#4081,#4082));
#696=EDGE_LOOP('',(#4083,#4084,#4085,#4086));
#697=EDGE_LOOP('',(#4087,#4088,#4089,#4090));
#698=EDGE_LOOP('',(#4091,#4092,#4093,#4094));
#699=EDGE_LOOP('',(#4095,#4096,#4097,#4098));
#700=EDGE_LOOP('',(#4099,#4100,#4101,#4102));
#701=EDGE_LOOP('',(#4103,#4104,#4105,#4106,#4107));
#702=EDGE_LOOP('',(#4108,#4109,#4110,#4111));
#703=EDGE_LOOP('',(#4112,#4113,#4114,#4115));
#704=EDGE_LOOP('',(#4116,#4117,#4118,#4119));
#705=EDGE_LOOP('',(#4120,#4121,#4122,#4123));
#706=EDGE_LOOP('',(#4124,#4125,#4126,#4127));
#707=EDGE_LOOP('',(#4128,#4129,#4130,#4131));
#708=EDGE_LOOP('',(#4132,#4133,#4134,#4135));
#709=EDGE_LOOP('',(#4136,#4137,#4138,#4139));
#710=EDGE_LOOP('',(#4140,#4141,#4142,#4143));
#711=EDGE_LOOP('',(#4144,#4145,#4146,#4147));
#712=EDGE_LOOP('',(#4148,#4149,#4150,#4151,#4152));
#713=EDGE_LOOP('',(#4153,#4154,#4155,#4156));
#714=EDGE_LOOP('',(#4157,#4158,#4159,#4160));
#715=EDGE_LOOP('',(#4161,#4162,#4163,#4164));
#716=EDGE_LOOP('',(#4165,#4166,#4167,#4168));
#717=EDGE_LOOP('',(#4169,#4170,#4171,#4172));
#718=EDGE_LOOP('',(#4173,#4174,#4175,#4176));
#719=EDGE_LOOP('',(#4177,#4178,#4179,#4180));
#720=EDGE_LOOP('',(#4181,#4182,#4183,#4184));
#721=EDGE_LOOP('',(#4185,#4186,#4187,#4188));
#722=EDGE_LOOP('',(#4189,#4190,#4191,#4192));
#723=EDGE_LOOP('',(#4193,#4194,#4195,#4196));
#724=EDGE_LOOP('',(#4197,#4198,#4199,#4200));
#725=EDGE_LOOP('',(#4201,#4202,#4203,#4204));
#726=EDGE_LOOP('',(#4205,#4206,#4207,#4208));
#727=EDGE_LOOP('',(#4209,#4210,#4211,#4212));
#728=EDGE_LOOP('',(#4213,#4214,#4215,#4216));
#729=EDGE_LOOP('',(#4217,#4218,#4219,#4220));
#730=EDGE_LOOP('',(#4221,#4222,#4223,#4224));
#731=EDGE_LOOP('',(#4225,#4226,#4227,#4228));
#732=EDGE_LOOP('',(#4229,#4230,#4231,#4232));
#733=EDGE_LOOP('',(#4233,#4234,#4235,#4236));
#734=EDGE_LOOP('',(#4237,#4238,#4239,#4240));
#735=EDGE_LOOP('',(#4241,#4242,#4243,#4244));
#736=EDGE_LOOP('',(#4245,#4246,#4247,#4248));
#737=EDGE_LOOP('',(#4249,#4250,#4251,#4252));
#738=EDGE_LOOP('',(#4253,#4254,#4255,#4256));
#739=EDGE_LOOP('',(#4257,#4258,#4259,#4260));
#740=EDGE_LOOP('',(#4261,#4262,#4263,#4264));
#741=EDGE_LOOP('',(#4265,#4266,#4267,#4268));
#742=EDGE_LOOP('',(#4269,#4270,#4271,#4272));
#743=EDGE_LOOP('',(#4273,#4274,#4275,#4276));
#744=EDGE_LOOP('',(#4277,#4278,#4279,#4280));
#745=EDGE_LOOP('',(#4281,#4282,#4283,#4284));
#746=EDGE_LOOP('',(#4285,#4286,#4287,#4288));
#747=EDGE_LOOP('',(#4289,#4290,#4291,#4292));
#748=EDGE_LOOP('',(#4293,#4294,#4295,#4296));
#749=EDGE_LOOP('',(#4297,#4298,#4299,#4300));
#750=EDGE_LOOP('',(#4301,#4302,#4303,#4304));
#751=EDGE_LOOP('',(#4305,#4306,#4307,#4308));
#752=EDGE_LOOP('',(#4309,#4310,#4311,#4312));
#753=EDGE_LOOP('',(#4313,#4314,#4315,#4316));
#754=EDGE_LOOP('',(#4317,#4318,#4319,#4320));
#755=EDGE_LOOP('',(#4321,#4322,#4323,#4324));
#756=EDGE_LOOP('',(#4325,#4326,#4327,#4328));
#757=EDGE_LOOP('',(#4329,#4330,#4331,#4332));
#758=EDGE_LOOP('',(#4333,#4334,#4335,#4336));
#759=EDGE_LOOP('',(#4337,#4338,#4339,#4340));
#760=EDGE_LOOP('',(#4341,#4342,#4343,#4344));
#761=EDGE_LOOP('',(#4345,#4346,#4347,#4348));
#762=EDGE_LOOP('',(#4349,#4350,#4351,#4352));
#763=EDGE_LOOP('',(#4353,#4354,#4355,#4356));
#764=EDGE_LOOP('',(#4357,#4358,#4359,#4360));
#765=EDGE_LOOP('',(#4361,#4362,#4363,#4364));
#766=EDGE_LOOP('',(#4365,#4366,#4367,#4368));
#767=EDGE_LOOP('',(#4369,#4370,#4371,#4372,#4373,#4374));
#768=EDGE_LOOP('',(#4375,#4376,#4377,#4378,#4379));
#769=EDGE_LOOP('',(#4380,#4381,#4382,#4383));
#770=EDGE_LOOP('',(#4384,#4385,#4386,#4387,#4388,#4389,#4390,#4391,#4392));
#771=EDGE_LOOP('',(#4393,#4394,#4395,#4396,#4397,#4398));
#772=EDGE_LOOP('',(#4399,#4400,#4401,#4402,#4403,#4404,#4405));
#773=EDGE_LOOP('',(#4406,#4407,#4408,#4409));
#774=EDGE_LOOP('',(#4410,#4411,#4412,#4413,#4414,#4415));
#775=EDGE_LOOP('',(#4416,#4417,#4418,#4419));
#776=EDGE_LOOP('',(#4420,#4421,#4422,#4423));
#777=EDGE_LOOP('',(#4424,#4425,#4426,#4427));
#778=EDGE_LOOP('',(#4428,#4429,#4430,#4431,#4432,#4433,#4434));
#779=EDGE_LOOP('',(#4435,#4436,#4437,#4438,#4439,#4440,#4441));
#780=EDGE_LOOP('',(#4442,#4443,#4444,#4445,#4446));
#781=EDGE_LOOP('',(#4447,#4448,#4449,#4450,#4451));
#782=EDGE_LOOP('',(#4452,#4453,#4454,#4455));
#783=EDGE_LOOP('',(#4456,#4457,#4458,#4459,#4460,#4461,#4462,#4463,#4464,
#4465,#4466,#4467,#4468,#4469,#4470,#4471,#4472,#4473,#4474,#4475,#4476,
#4477,#4478,#4479,#4480,#4481,#4482,#4483));
#784=EDGE_LOOP('',(#4484,#4485,#4486,#4487,#4488,#4489,#4490,#4491,#4492,
#4493,#4494,#4495,#4496,#4497,#4498,#4499,#4500,#4501,#4502,#4503,#4504,
#4505,#4506,#4507,#4508,#4509,#4510));
#785=EDGE_LOOP('',(#4511,#4512,#4513,#4514,#4515,#4516));
#786=EDGE_LOOP('',(#4517,#4518,#4519,#4520));
#787=EDGE_LOOP('',(#4521,#4522,#4523,#4524));
#788=EDGE_LOOP('',(#4525,#4526,#4527,#4528));
#789=EDGE_LOOP('',(#4529,#4530,#4531,#4532));
#790=EDGE_LOOP('',(#4533,#4534,#4535,#4536));
#791=EDGE_LOOP('',(#4537,#4538,#4539,#4540));
#792=EDGE_LOOP('',(#4541,#4542,#4543,#4544));
#793=EDGE_LOOP('',(#4545,#4546,#4547,#4548));
#794=EDGE_LOOP('',(#4549,#4550,#4551,#4552,#4553,#4554,#4555,#4556,#4557,
#4558,#4559,#4560,#4561,#4562,#4563,#4564,#4565,#4566,#4567,#4568,#4569,
#4570,#4571,#4572,#4573,#4574,#4575));
#795=EDGE_LOOP('',(#4576,#4577,#4578,#4579,#4580,#4581,#4582,#4583,#4584,
#4585,#4586,#4587,#4588,#4589,#4590,#4591,#4592,#4593,#4594,#4595,#4596,
#4597,#4598,#4599,#4600,#4601,#4602));
#796=EDGE_LOOP('',(#4603,#4604,#4605,#4606));
#797=EDGE_LOOP('',(#4607,#4608,#4609,#4610,#4611,#4612,#4613,#4614,#4615,
#4616,#4617,#4618,#4619,#4620,#4621,#4622,#4623,#4624,#4625,#4626,#4627,
#4628,#4629,#4630,#4631,#4632,#4633));
#798=EDGE_LOOP('',(#4634,#4635,#4636,#4637,#4638,#4639,#4640,#4641,#4642,
#4643,#4644,#4645,#4646,#4647,#4648,#4649,#4650,#4651,#4652,#4653,#4654,
#4655,#4656,#4657,#4658,#4659,#4660));
#799=EDGE_LOOP('',(#4661,#4662,#4663,#4664));
#800=EDGE_LOOP('',(#4665,#4666,#4667,#4668,#4669,#4670,#4671,#4672,#4673,
#4674,#4675,#4676,#4677,#4678,#4679,#4680,#4681,#4682,#4683,#4684,#4685,
#4686,#4687,#4688,#4689,#4690,#4691));
#801=EDGE_LOOP('',(#4692,#4693,#4694,#4695,#4696,#4697,#4698,#4699,#4700,
#4701,#4702,#4703,#4704,#4705,#4706,#4707,#4708,#4709,#4710,#4711,#4712,
#4713,#4714,#4715,#4716,#4717,#4718,#4719));
#802=EDGE_LOOP('',(#4720,#4721,#4722,#4723,#4724,#4725,#4726,#4727,#4728,
#4729));
#803=EDGE_LOOP('',(#4730,#4731,#4732,#4733));
#804=EDGE_LOOP('',(#4734,#4735,#4736,#4737));
#805=EDGE_LOOP('',(#4738,#4739,#4740,#4741));
#806=EDGE_LOOP('',(#4742,#4743,#4744,#4745,#4746,#4747));
#807=EDGE_LOOP('',(#4748,#4749,#4750,#4751));
#808=EDGE_LOOP('',(#4752,#4753,#4754,#4755,#4756,#4757));
#809=EDGE_LOOP('',(#4758,#4759,#4760,#4761));
#810=EDGE_LOOP('',(#4762,#4763,#4764,#4765));
#811=EDGE_LOOP('',(#4766,#4767,#4768,#4769));
#812=EDGE_LOOP('',(#4770,#4771,#4772,#4773));
#813=EDGE_LOOP('',(#4774,#4775,#4776,#4777));
#814=EDGE_LOOP('',(#4778,#4779,#4780,#4781));
#815=EDGE_LOOP('',(#4782,#4783,#4784,#4785));
#816=EDGE_LOOP('',(#4786,#4787,#4788,#4789));
#817=EDGE_LOOP('',(#4790,#4791,#4792,#4793));
#818=EDGE_LOOP('',(#4794,#4795,#4796,#4797));
#819=EDGE_LOOP('',(#4798,#4799,#4800,#4801));
#820=EDGE_LOOP('',(#4802,#4803,#4804,#4805));
#821=EDGE_LOOP('',(#4806,#4807,#4808,#4809));
#822=EDGE_LOOP('',(#4810,#4811,#4812,#4813));
#823=EDGE_LOOP('',(#4814,#4815,#4816,#4817));
#824=EDGE_LOOP('',(#4818,#4819,#4820,#4821));
#825=EDGE_LOOP('',(#4822,#4823,#4824,#4825));
#826=EDGE_LOOP('',(#4826,#4827,#4828,#4829));
#827=EDGE_LOOP('',(#4830));
#828=EDGE_LOOP('',(#4831));
#829=EDGE_LOOP('',(#4832,#4833,#4834,#4835,#4836,#4837));
#830=EDGE_LOOP('',(#4838,#4839,#4840,#4841));
#831=EDGE_LOOP('',(#4842,#4843,#4844,#4845));
#832=EDGE_LOOP('',(#4846,#4847,#4848,#4849));
#833=EDGE_LOOP('',(#4850,#4851,#4852,#4853));
#834=EDGE_LOOP('',(#4854,#4855,#4856,#4857));
#835=EDGE_LOOP('',(#4858,#4859,#4860,#4861));
#836=EDGE_LOOP('',(#4862,#4863,#4864,#4865));
#837=EDGE_LOOP('',(#4866,#4867,#4868,#4869,#4870));
#838=EDGE_LOOP('',(#4871,#4872,#4873,#4874));
#839=EDGE_LOOP('',(#4875,#4876,#4877,#4878));
#840=EDGE_LOOP('',(#4879,#4880,#4881,#4882));
#841=EDGE_LOOP('',(#4883,#4884,#4885));
#842=EDGE_LOOP('',(#4886,#4887,#4888));
#843=EDGE_LOOP('',(#4889,#4890,#4891));
#844=EDGE_LOOP('',(#4892,#4893,#4894));
#845=EDGE_LOOP('',(#4895,#4896,#4897));
#846=EDGE_LOOP('',(#4898,#4899,#4900));
#847=EDGE_LOOP('',(#4901,#4902,#4903));
#848=EDGE_LOOP('',(#4904,#4905,#4906));
#849=EDGE_LOOP('',(#4907,#4908,#4909,#4910));
#850=EDGE_LOOP('',(#4911,#4912,#4913,#4914));
#851=EDGE_LOOP('',(#4915,#4916,#4917,#4918));
#852=EDGE_LOOP('',(#4919,#4920,#4921,#4922));
#853=EDGE_LOOP('',(#4923,#4924,#4925,#4926));
#854=EDGE_LOOP('',(#4927,#4928,#4929,#4930));
#855=EDGE_LOOP('',(#4931,#4932,#4933,#4934));
#856=EDGE_LOOP('',(#4935,#4936,#4937,#4938));
#857=EDGE_LOOP('',(#4939,#4940,#4941,#4942));
#858=EDGE_LOOP('',(#4943,#4944,#4945,#4946));
#859=EDGE_LOOP('',(#4947,#4948,#4949,#4950));
#860=EDGE_LOOP('',(#4951,#4952,#4953,#4954));
#861=EDGE_LOOP('',(#4955,#4956,#4957,#4958));
#862=EDGE_LOOP('',(#4959,#4960,#4961,#4962));
#863=EDGE_LOOP('',(#4963,#4964,#4965,#4966));
#864=EDGE_LOOP('',(#4967));
#865=EDGE_LOOP('',(#4968));
#866=EDGE_LOOP('',(#4969,#4970,#4971,#4972));
#867=EDGE_LOOP('',(#4973,#4974,#4975,#4976));
#868=EDGE_LOOP('',(#4977,#4978,#4979,#4980));
#869=EDGE_LOOP('',(#4981,#4982,#4983,#4984));
#870=EDGE_LOOP('',(#4985));
#871=EDGE_LOOP('',(#4986));
#872=EDGE_LOOP('',(#4987,#4988,#4989,#4990));
#873=EDGE_LOOP('',(#4991,#4992,#4993,#4994));
#874=EDGE_LOOP('',(#4995,#4996,#4997,#4998));
#875=EDGE_LOOP('',(#4999,#5000,#5001,#5002));
#876=EDGE_LOOP('',(#5003,#5004,#5005,#5006));
#877=EDGE_LOOP('',(#5007,#5008,#5009,#5010));
#878=EDGE_LOOP('',(#5011,#5012,#5013,#5014));
#879=EDGE_LOOP('',(#5015,#5016,#5017,#5018));
#880=EDGE_LOOP('',(#5019,#5020,#5021,#5022));
#881=EDGE_LOOP('',(#5023,#5024,#5025,#5026));
#882=EDGE_LOOP('',(#5027,#5028,#5029,#5030));
#883=EDGE_LOOP('',(#5031,#5032,#5033,#5034));
#884=EDGE_LOOP('',(#5035,#5036,#5037,#5038));
#885=EDGE_LOOP('',(#5039,#5040,#5041,#5042));
#886=EDGE_LOOP('',(#5043,#5044,#5045,#5046));
#887=EDGE_LOOP('',(#5047,#5048,#5049,#5050));
#888=EDGE_LOOP('',(#5051,#5052,#5053,#5054));
#889=EDGE_LOOP('',(#5055,#5056,#5057,#5058));
#890=EDGE_LOOP('',(#5059));
#891=EDGE_LOOP('',(#5060));
#892=EDGE_LOOP('',(#5061,#5062,#5063,#5064));
#893=EDGE_LOOP('',(#5065,#5066,#5067,#5068));
#894=EDGE_LOOP('',(#5069));
#895=EDGE_LOOP('',(#5070));
#896=EDGE_LOOP('',(#5071,#5072,#5073,#5074));
#897=EDGE_LOOP('',(#5075,#5076,#5077,#5078));
#898=EDGE_LOOP('',(#5079,#5080,#5081,#5082));
#899=EDGE_LOOP('',(#5083,#5084,#5085,#5086));
#900=EDGE_LOOP('',(#5087,#5088,#5089,#5090));
#901=EDGE_LOOP('',(#5091,#5092,#5093,#5094));
#902=EDGE_LOOP('',(#5095,#5096,#5097,#5098));
#903=EDGE_LOOP('',(#5099,#5100,#5101,#5102));
#904=EDGE_LOOP('',(#5103,#5104,#5105,#5106));
#905=EDGE_LOOP('',(#5107,#5108,#5109,#5110));
#906=EDGE_LOOP('',(#5111,#5112,#5113,#5114));
#907=EDGE_LOOP('',(#5115,#5116,#5117,#5118));
#908=EDGE_LOOP('',(#5119,#5120,#5121,#5122));
#909=EDGE_LOOP('',(#5123,#5124,#5125,#5126));
#910=EDGE_LOOP('',(#5127,#5128,#5129,#5130));
#911=EDGE_LOOP('',(#5131,#5132,#5133,#5134));
#912=EDGE_LOOP('',(#5135,#5136,#5137,#5138));
#913=EDGE_LOOP('',(#5139,#5140,#5141,#5142));
#914=EDGE_LOOP('',(#5143,#5144,#5145,#5146));
#915=EDGE_LOOP('',(#5147,#5148,#5149,#5150));
#916=EDGE_LOOP('',(#5151,#5152,#5153,#5154));
#917=EDGE_LOOP('',(#5155,#5156,#5157,#5158));
#918=EDGE_LOOP('',(#5159,#5160,#5161,#5162));
#919=EDGE_LOOP('',(#5163,#5164,#5165,#5166));
#920=EDGE_LOOP('',(#5167,#5168,#5169,#5170));
#921=EDGE_LOOP('',(#5171));
#922=EDGE_LOOP('',(#5172));
#923=EDGE_LOOP('',(#5173));
#924=EDGE_LOOP('',(#5174));
#925=EDGE_LOOP('',(#5175,#5176,#5177,#5178));
#926=EDGE_LOOP('',(#5179,#5180,#5181,#5182));
#927=EDGE_LOOP('',(#5183,#5184,#5185,#5186));
#928=EDGE_LOOP('',(#5187,#5188,#5189,#5190));
#929=EDGE_LOOP('',(#5191));
#930=EDGE_LOOP('',(#5192));
#931=EDGE_LOOP('',(#5193));
#932=EDGE_LOOP('',(#5194));
#933=EDGE_LOOP('',(#5195,#5196,#5197,#5198));
#934=EDGE_LOOP('',(#5199,#5200,#5201,#5202));
#935=EDGE_LOOP('',(#5203));
#936=EDGE_LOOP('',(#5204,#5205,#5206,#5207));
#937=EDGE_LOOP('',(#5208,#5209,#5210,#5211));
#938=EDGE_LOOP('',(#5212));
#939=EDGE_LOOP('',(#5213,#5214,#5215,#5216));
#940=EDGE_LOOP('',(#5217,#5218,#5219,#5220));
#941=EDGE_LOOP('',(#5221,#5222,#5223,#5224));
#942=EDGE_LOOP('',(#5225,#5226,#5227,#5228));
#943=EDGE_LOOP('',(#5229,#5230,#5231,#5232));
#944=EDGE_LOOP('',(#5233));
#945=EDGE_LOOP('',(#5234,#5235,#5236,#5237));
#946=EDGE_LOOP('',(#5238,#5239,#5240,#5241));
#947=EDGE_LOOP('',(#5242));
#948=EDGE_LOOP('',(#5243,#5244,#5245,#5246));
#949=EDGE_LOOP('',(#5247,#5248,#5249,#5250));
#950=EDGE_LOOP('',(#5251,#5252,#5253,#5254));
#951=EDGE_LOOP('',(#5255,#5256,#5257,#5258));
#952=EDGE_LOOP('',(#5259,#5260,#5261,#5262));
#953=EDGE_LOOP('',(#5263,#5264,#5265,#5266));
#954=EDGE_LOOP('',(#5267,#5268,#5269,#5270));
#955=EDGE_LOOP('',(#5271,#5272,#5273,#5274));
#956=EDGE_LOOP('',(#5275,#5276,#5277,#5278));
#957=EDGE_LOOP('',(#5279,#5280,#5281,#5282));
#958=EDGE_LOOP('',(#5283,#5284,#5285,#5286));
#959=EDGE_LOOP('',(#5287,#5288,#5289,#5290));
#960=EDGE_LOOP('',(#5291,#5292,#5293,#5294));
#961=EDGE_LOOP('',(#5295,#5296,#5297,#5298));
#962=EDGE_LOOP('',(#5299,#5300,#5301,#5302));
#963=EDGE_LOOP('',(#5303,#5304,#5305,#5306));
#964=EDGE_LOOP('',(#5307,#5308,#5309,#5310));
#965=EDGE_LOOP('',(#5311,#5312,#5313,#5314));
#966=EDGE_LOOP('',(#5315,#5316,#5317,#5318));
#967=EDGE_LOOP('',(#5319,#5320,#5321,#5322));
#968=EDGE_LOOP('',(#5323,#5324,#5325,#5326));
#969=EDGE_LOOP('',(#5327,#5328,#5329,#5330));
#970=EDGE_LOOP('',(#5331,#5332,#5333,#5334));
#971=EDGE_LOOP('',(#5335,#5336,#5337,#5338,#5339,#5340,#5341,#5342));
#972=EDGE_LOOP('',(#5343,#5344,#5345,#5346,#5347,#5348,#5349,#5350,#5351,
#5352,#5353,#5354,#5355,#5356,#5357,#5358,#5359,#5360,#5361,#5362,#5363,
#5364,#5365,#5366));
#973=EDGE_LOOP('',(#5367,#5368,#5369,#5370));
#974=EDGE_LOOP('',(#5371,#5372,#5373,#5374,#5375,#5376,#5377,#5378,#5379,
#5380,#5381,#5382,#5383,#5384,#5385,#5386,#5387,#5388,#5389,#5390,#5391,
#5392,#5393,#5394,#5395));
#975=EDGE_LOOP('',(#5396,#5397,#5398,#5399));
#976=EDGE_LOOP('',(#5400,#5401,#5402,#5403));
#977=EDGE_LOOP('',(#5404,#5405,#5406,#5407));
#978=EDGE_LOOP('',(#5408,#5409,#5410,#5411));
#979=EDGE_LOOP('',(#5412,#5413,#5414,#5415));
#980=EDGE_LOOP('',(#5416,#5417,#5418,#5419));
#981=EDGE_LOOP('',(#5420,#5421,#5422,#5423));
#982=EDGE_LOOP('',(#5424,#5425,#5426,#5427,#5428,#5429));
#983=EDGE_LOOP('',(#5430));
#984=EDGE_LOOP('',(#5431,#5432,#5433,#5434));
#985=EDGE_LOOP('',(#5435,#5436,#5437,#5438));
#986=EDGE_LOOP('',(#5439));
#987=EDGE_LOOP('',(#5440,#5441,#5442,#5443,#5444,#5445));
#988=EDGE_LOOP('',(#5446));
#989=EDGE_LOOP('',(#5447,#5448,#5449,#5450));
#990=EDGE_LOOP('',(#5451,#5452,#5453,#5454));
#991=EDGE_LOOP('',(#5455,#5456,#5457,#5458));
#992=EDGE_LOOP('',(#5459,#5460,#5461,#5462));
#993=EDGE_LOOP('',(#5463,#5464,#5465,#5466));
#994=EDGE_LOOP('',(#5467,#5468,#5469,#5470));
#995=EDGE_LOOP('',(#5471,#5472,#5473,#5474));
#996=EDGE_LOOP('',(#5475,#5476,#5477,#5478));
#997=EDGE_LOOP('',(#5479,#5480,#5481,#5482));
#998=EDGE_LOOP('',(#5483,#5484,#5485,#5486));
#999=EDGE_LOOP('',(#5487,#5488,#5489,#5490));
#1000=EDGE_LOOP('',(#5491,#5492,#5493,#5494));
#1001=EDGE_LOOP('',(#5495,#5496,#5497,#5498));
#1002=EDGE_LOOP('',(#5499,#5500,#5501,#5502));
#1003=EDGE_LOOP('',(#5503,#5504,#5505,#5506));
#1004=EDGE_LOOP('',(#5507,#5508,#5509,#5510));
#1005=EDGE_LOOP('',(#5511,#5512,#5513,#5514));
#1006=EDGE_LOOP('',(#5515,#5516,#5517,#5518));
#1007=EDGE_LOOP('',(#5519,#5520,#5521,#5522));
#1008=EDGE_LOOP('',(#5523,#5524,#5525,#5526));
#1009=EDGE_LOOP('',(#5527,#5528,#5529,#5530));
#1010=EDGE_LOOP('',(#5531,#5532,#5533,#5534));
#1011=EDGE_LOOP('',(#5535,#5536,#5537,#5538));
#1012=EDGE_LOOP('',(#5539,#5540,#5541,#5542));
#1013=EDGE_LOOP('',(#5543,#5544,#5545,#5546));
#1014=EDGE_LOOP('',(#5547,#5548,#5549,#5550));
#1015=EDGE_LOOP('',(#5551,#5552,#5553,#5554));
#1016=EDGE_LOOP('',(#5555,#5556,#5557,#5558));
#1017=EDGE_LOOP('',(#5559,#5560,#5561,#5562));
#1018=EDGE_LOOP('',(#5563,#5564,#5565,#5566));
#1019=EDGE_LOOP('',(#5567,#5568,#5569,#5570,#5571,#5572,#5573,#5574));
#1020=EDGE_LOOP('',(#5575,#5576,#5577,#5578,#5579,#5580,#5581,#5582,#5583,
#5584,#5585,#5586,#5587,#5588,#5589,#5590,#5591,#5592,#5593,#5594,#5595,
#5596,#5597,#5598,#5599,#5600,#5601,#5602,#5603,#5604,#5605,#5606,#5607,
#5608));
#1021=EDGE_LOOP('',(#5609,#5610,#5611,#5612));
#1022=EDGE_LOOP('',(#5613,#5614,#5615,#5616,#5617,#5618,#5619,#5620,#5621,
#5622,#5623,#5624,#5625,#5626,#5627,#5628,#5629,#5630,#5631,#5632,#5633,
#5634,#5635,#5636,#5637,#5638,#5639,#5640,#5641,#5642,#5643,#5644,#5645,
#5646,#5647));
#1023=EDGE_LOOP('',(#5648,#5649,#5650,#5651));
#1024=EDGE_LOOP('',(#5652,#5653,#5654,#5655));
#1025=EDGE_LOOP('',(#5656,#5657,#5658,#5659));
#1026=EDGE_LOOP('',(#5660,#5661,#5662,#5663));
#1027=EDGE_LOOP('',(#5664,#5665,#5666,#5667));
#1028=EDGE_LOOP('',(#5668,#5669,#5670,#5671));
#1029=EDGE_LOOP('',(#5672,#5673,#5674,#5675));
#1030=EDGE_LOOP('',(#5676,#5677,#5678,#5679,#5680,#5681));
#1031=EDGE_LOOP('',(#5682));
#1032=EDGE_LOOP('',(#5683,#5684,#5685,#5686));
#1033=EDGE_LOOP('',(#5687,#5688,#5689,#5690));
#1034=EDGE_LOOP('',(#5691));
#1035=EDGE_LOOP('',(#5692,#5693,#5694,#5695,#5696,#5697));
#1036=EDGE_LOOP('',(#5698));
#1037=EDGE_LOOP('',(#5699,#5700,#5701,#5702));
#1038=EDGE_LOOP('',(#5703,#5704,#5705,#5706));
#1039=EDGE_LOOP('',(#5707));
#1040=EDGE_LOOP('',(#5708));
#1041=EDGE_LOOP('',(#5709));
#1042=EDGE_LOOP('',(#5710));
#1043=EDGE_LOOP('',(#5711,#5712,#5713,#5714));
#1044=EDGE_LOOP('',(#5715,#5716,#5717,#5718));
#1045=EDGE_LOOP('',(#5719,#5720,#5721,#5722));
#1046=EDGE_LOOP('',(#5723,#5724,#5725,#5726));
#1047=EDGE_LOOP('',(#5727,#5728,#5729,#5730));
#1048=EDGE_LOOP('',(#5731,#5732,#5733,#5734));
#1049=EDGE_LOOP('',(#5735,#5736,#5737,#5738));
#1050=EDGE_LOOP('',(#5739,#5740,#5741,#5742));
#1051=EDGE_LOOP('',(#5743,#5744,#5745,#5746));
#1052=EDGE_LOOP('',(#5747,#5748,#5749,#5750));
#1053=EDGE_LOOP('',(#5751,#5752,#5753,#5754));
#1054=EDGE_LOOP('',(#5755,#5756,#5757,#5758,#5759,#5760,#5761,#5762,#5763,
#5764,#5765,#5766,#5767,#5768));
#1055=EDGE_LOOP('',(#5769,#5770,#5771,#5772,#5773,#5774,#5775,#5776,#5777,
#5778,#5779,#5780,#5781,#5782));
#1056=EDGE_LOOP('',(#5783,#5784,#5785,#5786,#5787,#5788));
#1057=EDGE_LOOP('',(#5789,#5790,#5791,#5792));
#1058=EDGE_LOOP('',(#5793,#5794,#5795,#5796));
#1059=EDGE_LOOP('',(#5797,#5798,#5799,#5800));
#1060=EDGE_LOOP('',(#5801,#5802,#5803,#5804));
#1061=EDGE_LOOP('',(#5805,#5806,#5807,#5808));
#1062=EDGE_LOOP('',(#5809,#5810,#5811,#5812));
#1063=EDGE_LOOP('',(#5813,#5814,#5815,#5816));
#1064=EDGE_LOOP('',(#5817,#5818,#5819,#5820));
#1065=EDGE_LOOP('',(#5821,#5822,#5823,#5824,#5825,#5826));
#1066=EDGE_LOOP('',(#5827,#5828,#5829,#5830));
#1067=CIRCLE('',#6505,1.666);
#1068=CIRCLE('',#6516,1.666);
#1069=CIRCLE('',#6518,1.666);
#1070=CIRCLE('',#6529,1.666);
#1071=CIRCLE('',#6531,1.666);
#1072=CIRCLE('',#6542,1.666);
#1073=CIRCLE('',#6543,1.666);
#1074=CIRCLE('',#6545,1.666);
#1075=CIRCLE('',#6556,1.666);
#1076=CIRCLE('',#6557,1.666);
#1077=CIRCLE('',#6559,2.05475);
#1078=CIRCLE('',#6571,2.05475);
#1079=CIRCLE('',#6573,2.05475);
#1080=CIRCLE('',#6585,2.05475);
#1081=CIRCLE('',#6587,2.05475);
#1082=CIRCLE('',#6599,2.05475);
#1083=CIRCLE('',#6601,2.05475);
#1084=CIRCLE('',#6613,2.05475);
#1085=CIRCLE('',#6630,5.5);
#1086=CIRCLE('',#6631,5.5);
#1087=CIRCLE('',#6632,5.5);
#1088=CIRCLE('',#6644,2.);
#1089=CIRCLE('',#6645,3.5);
#1090=CIRCLE('',#6646,3.5);
#1091=CIRCLE('',#6648,2.);
#1092=CIRCLE('',#6649,3.5);
#1093=CIRCLE('',#6650,3.5);
#1094=CIRCLE('',#6652,3.5);
#1095=CIRCLE('',#6654,3.5);
#1096=CIRCLE('',#6695,1.);
#1097=CIRCLE('',#6696,0.999999999999996);
#1098=CIRCLE('',#6697,1.);
#1099=CIRCLE('',#6699,1.);
#1100=CIRCLE('',#6700,0.999999999999996);
#1101=CIRCLE('',#6701,1.);
#1102=CIRCLE('',#6703,0.999999999999996);
#1103=CIRCLE('',#6704,1.);
#1104=CIRCLE('',#6705,1.);
#1105=CIRCLE('',#6707,1.);
#1106=CIRCLE('',#6708,0.999999999999996);
#1107=CIRCLE('',#6709,1.);
#1108=CIRCLE('',#6711,1.);
#1109=CIRCLE('',#6712,1.);
#1110=CIRCLE('',#6713,0.999999999999996);
#1111=CIRCLE('',#6715,1.);
#1112=CIRCLE('',#6716,0.999999999999996);
#1113=CIRCLE('',#6717,1.);
#1114=CIRCLE('',#6719,0.999999999999996);
#1115=CIRCLE('',#6720,1.);
#1116=CIRCLE('',#6721,1.);
#1117=CIRCLE('',#6723,0.999999999999996);
#1118=CIRCLE('',#6724,1.);
#1119=CIRCLE('',#6725,1.);
#1120=CIRCLE('',#6740,3.5);
#1121=CIRCLE('',#6741,3.5);
#1122=CIRCLE('',#6745,3.5);
#1123=CIRCLE('',#6746,3.5);
#1124=CIRCLE('',#6756,3.5);
#1125=CIRCLE('',#6757,3.5);
#1126=CIRCLE('',#6759,3.5);
#1127=CIRCLE('',#6760,3.5);
#1128=CIRCLE('',#6773,2.5);
#1129=CIRCLE('',#6774,2.5);
#1130=CIRCLE('',#6776,2.5);
#1131=CIRCLE('',#6777,2.5);
#1132=CIRCLE('',#6779,2.5);
#1133=CIRCLE('',#6780,2.5);
#1134=CIRCLE('',#6782,2.5);
#1135=CIRCLE('',#6783,2.5);
#1136=CIRCLE('',#6804,1.);
#1137=CIRCLE('',#6805,1.);
#1138=CIRCLE('',#6814,1.);
#1139=CIRCLE('',#6815,1.);
#1140=CIRCLE('',#6824,1.954);
#1141=CIRCLE('',#6835,1.5555);
#1142=CIRCLE('',#6846,1.954);
#1143=CIRCLE('',#6847,1.);
#1144=CIRCLE('',#6849,1.5555);
#1145=CIRCLE('',#6859,3.5);
#1146=CIRCLE('',#6861,3.5);
#1147=CIRCLE('',#6866,2.942);
#1148=CIRCLE('',#6882,2.37175);
#1149=CIRCLE('',#6898,2.942);
#1150=CIRCLE('',#6899,2.);
#1151=CIRCLE('',#6901,2.37175);
#1152=CIRCLE('',#6911,5.);
#1153=CIRCLE('',#6913,5.);
#1154=CIRCLE('',#6918,3.5);
#1155=CIRCLE('',#6919,3.5);
#1156=CIRCLE('',#6921,7.);
#1157=CIRCLE('',#6922,7.);
#1158=CIRCLE('',#6927,2.5175);
#1159=CIRCLE('',#6932,2.5175);
#1160=CIRCLE('',#6934,3.0735);
#1161=CIRCLE('',#6939,3.0735);
#1162=B_SPLINE_CURVE_WITH_KNOTS('',3,(#8360,#8361,#8362,#8363,#8364,#8365,
#8366,#8367,#8368,#8369,#8370,#8371,#8372),.UNSPECIFIED.,.F.,.F.,(4,3,3,
3,4),(70.4248606341474,70.8296431251379,71.8272437325342,72.8248443399306,
73.8224449473268),.UNSPECIFIED.);
#1163=B_SPLINE_CURVE_WITH_KNOTS('',3,(#8375,#8376,#8377,#8378,#8379,#8380,
#8381,#8382,#8383,#8384,#8385,#8386,#8387,#8388,#8389,#8390,#8391,#8392,
#8393),.UNSPECIFIED.,.F.,.F.,(4,3,3,3,3,3,4),(-71.8078320820524,-70.829643125138,
-69.8320425177416,-68.8344419103453,-67.836841302949,-66.8392406955527,
-66.6782363354882),.UNSPECIFIED.);
#1164=B_SPLINE_CURVE_WITH_KNOTS('',3,(#8398,#8399,#8400,#8401,#8402,#8403,
#8404,#8405,#8406,#8407,#8408,#8409,#8410,#8411,#8412,#8413,#8414,#8415,
#8416,#8417,#8418,#8419),.UNSPECIFIED.,.F.,.F.,(4,3,3,3,3,3,3,4),(64.1416753269678,
64.8440394807601,65.8416400881564,66.8392406955527,67.836841302949,68.8344419103453,
69.8320425177416,70.4248606341474),.UNSPECIFIED.);
#1165=B_SPLINE_CURVE_WITH_KNOTS('',3,(#8420,#8421,#8422,#8423,#8424,#8425,
#8426,#8427,#8428,#8429,#8430,#8431,#8432,#8433,#8434,#8435,#8436,#8437,
#8438,#8439,#8440,#8441),.UNSPECIFIED.,.F.,.F.,(4,3,3,3,3,3,3,4),(-66.6782363354882,
-65.8416400881564,-64.8440394807601,-63.8464388733638,-62.8488382659675,
-61.8512376585712,-60.8536370511749,-60.3950510283086),.UNSPECIFIED.);
#1166=B_SPLINE_CURVE_WITH_KNOTS('',3,(#8446,#8447,#8448,#8449,#8450,#8451,
#8452,#8453,#8454,#8455,#8456,#8457,#8458,#8459,#8460,#8461,#8462,#8463,
#8464,#8465,#8466,#8467),.UNSPECIFIED.,.F.,.F.,(4,3,3,3,3,3,3,4),(57.8584900197882,
58.8584358363822,59.8560364437785,60.8536370511749,61.8512376585712,62.8488382659675,
63.8464388733638,64.1416753269678),.UNSPECIFIED.);
#1167=B_SPLINE_CURVE_WITH_KNOTS('',3,(#8468,#8469,#8470,#8471,#8472,#8473,
#8474,#8475,#8476,#8477,#8478,#8479,#8480,#8481,#8482,#8483,#8484,#8485,
#8486,#8487,#8488,#8489),.UNSPECIFIED.,.F.,.F.,(4,3,3,3,3,3,3,4),(-60.3950510283086,
-59.8560364437785,-58.8584358363822,-57.8608352289859,-56.8632346215896,
-55.8656340141933,-54.868033406797,-54.111865721129),.UNSPECIFIED.);
#1168=B_SPLINE_CURVE_WITH_KNOTS('',3,(#8494,#8495,#8496,#8497,#8498,#8499,
#8500,#8501,#8502,#8503,#8504,#8505,#8506,#8507,#8508,#8509,#8510,#8511,
#8512,#8513,#8514,#8515),.UNSPECIFIED.,.F.,.F.,(4,3,3,3,3,3,3,4),(51.5753047126087,
51.8752315846081,52.8728321920044,53.8704327994007,54.868033406797,55.8656340141933,
56.8632346215896,57.8584900197882),.UNSPECIFIED.);
#1169=B_SPLINE_CURVE_WITH_KNOTS('',3,(#8516,#8517,#8518,#8519,#8520,#8521,
#8522,#8523,#8524,#8525,#8526,#8527,#8528,#8529,#8530,#8531,#8532,#8533,
#8534,#8535,#8536,#8537,#8538,#8539,#8540),.UNSPECIFIED.,.F.,.F.,(4,3,3,
3,3,3,3,3,4),(-54.111865721129,-53.8704327994007,-52.8728321920044,-51.8752315846081,
-50.8776309772118,-49.8800303698155,-48.8824297624191,-47.8848291550228,
-47.8286804139494),.UNSPECIFIED.);
#1170=B_SPLINE_CURVE_WITH_KNOTS('',3,(#8545,#8546,#8547,#8548,#8549,#8550,
#8551,#8552,#8553,#8554,#8555,#8556,#8557,#8558,#8559,#8560,#8561,#8562,
#8563,#8564,#8565,#8566),.UNSPECIFIED.,.F.,.F.,(4,3,3,3,3,3,3,4),(45.2921194054291,
45.8896279402302,46.8872285476265,47.8848291550228,48.8824297624192,49.8800303698155,
50.8776309772118,51.5753047126087),.UNSPECIFIED.);
#1171=B_SPLINE_CURVE_WITH_KNOTS('',3,(#8567,#8568,#8569,#8570,#8571,#8572,
#8573,#8574,#8575,#8576,#8577,#8578,#8579,#8580,#8581,#8582,#8583,#8584,
#8585,#8586,#8587,#8588),.UNSPECIFIED.,.F.,.F.,(4,3,3,3,3,3,3,4),(-47.8286804139494,
-46.8872285476265,-45.8896279402302,-44.8920273328339,-43.8944267254376,
-42.8968261180413,-41.899225510645,-41.5454951067698),.UNSPECIFIED.);
#1172=B_SPLINE_CURVE_WITH_KNOTS('',3,(#8593,#8594,#8595,#8596,#8597,#8598,
#8599,#8600,#8601,#8602,#8603,#8604,#8605,#8606,#8607,#8608,#8609,#8610,
#8611,#8612,#8613,#8614),.UNSPECIFIED.,.F.,.F.,(4,3,3,3,3,3,3,4),(39.0089340982495,
39.9040242958524,40.9016249032487,41.899225510645,42.8968261180413,43.8944267254376,
44.8920273328339,45.2921194054291),.UNSPECIFIED.);
#1173=B_SPLINE_CURVE_WITH_KNOTS('',3,(#8615,#8616,#8617,#8618,#8619,#8620,
#8621,#8622,#8623,#8624,#8625,#8626,#8627,#8628,#8629,#8630,#8631,#8632,
#8633,#8634,#8635,#8636),.UNSPECIFIED.,.F.,.F.,(4,3,3,3,3,3,3,4),(-41.5454951067698,
-40.9016249032487,-39.9040242958524,-38.9064236884561,-37.9088230810597,
-36.9112224736634,-35.9136218662671,-35.2623097995902),.UNSPECIFIED.);
#1174=B_SPLINE_CURVE_WITH_KNOTS('',3,(#8641,#8642,#8643,#8644,#8645,#8646,
#8647,#8648,#8649,#8650,#8651,#8652,#8653,#8654,#8655,#8656,#8657,#8658,
#8659,#8660,#8661,#8662,#8663,#8664,#8665),.UNSPECIFIED.,.F.,.F.,(4,3,3,
3,3,3,3,3,4),(32.7257487910699,32.9208200440782,33.9184206514745,34.9160212588708,
35.9136218662671,36.9112224736634,37.9088230810598,38.9064236884561,39.0089340982495),
 .UNSPECIFIED.);
#1175=B_SPLINE_CURVE_WITH_KNOTS('',3,(#8666,#8667,#8668,#8669,#8670,#8671,
#8672,#8673,#8674,#8675,#8676,#8677,#8678,#8679,#8680,#8681,#8682,#8683,
#8684,#8685,#8686,#8687),.UNSPECIFIED.,.F.,.F.,(4,3,3,3,3,3,3,4),(-35.2623097995902,
-34.9160212588708,-33.9184206514745,-32.9208200440782,-31.9232194366819,
-30.9256188292856,-29.9280182218893,-28.9791244924106),.UNSPECIFIED.);
#1176=B_SPLINE_CURVE_WITH_KNOTS('',3,(#8692,#8693,#8694,#8695,#8696,#8697,
#8698,#8699,#8700,#8701,#8702,#8703,#8704,#8705,#8706,#8707,#8708,#8709,
#8710,#8711,#8712,#8713),.UNSPECIFIED.,.F.,.F.,(4,3,3,3,3,3,3,4),(26.4425634838903,
26.9352163997003,27.9328170070967,28.930417614493,29.9280182218893,30.9256188292856,
31.9232194366819,32.7257487910699),.UNSPECIFIED.);
#1177=B_SPLINE_CURVE_WITH_KNOTS('',3,(#8714,#8715,#8716,#8717,#8718,#8719,
#8720,#8721,#8722,#8723,#8724,#8725,#8726,#8727,#8728,#8729,#8730,#8731,
#8732,#8733,#8734,#8735,#8736,#8737,#8738),.UNSPECIFIED.,.F.,.F.,(4,3,3,
3,3,3,3,3,4),(-28.9791244924106,-28.930417614493,-27.9328170070967,-26.9352163997003,
-25.937615792304,-24.9400151849077,-23.9424145775114,-22.9448139701151,
-22.695939185231),.UNSPECIFIED.);
#1178=B_SPLINE_CURVE_WITH_KNOTS('',3,(#8743,#8744,#8745,#8746,#8747,#8748,
#8749,#8750,#8751,#8752,#8753,#8754,#8755,#8756,#8757,#8758,#8759,#8760,
#8761,#8762,#8763,#8764),.UNSPECIFIED.,.F.,.F.,(4,3,3,3,3,3,3,4),(20.1593781767107,
20.9496127553225,21.9472133627188,22.9448139701151,23.9424145775114,24.9400151849077,
25.937615792304,26.4425634838903),.UNSPECIFIED.);
#1179=B_SPLINE_CURVE_WITH_KNOTS('',3,(#8765,#8766,#8767,#8768,#8769,#8770,
#8771,#8772,#8773,#8774,#8775,#8776,#8777,#8778,#8779,#8780,#8781,#8782,
#8783,#8784,#8785,#8786),.UNSPECIFIED.,.F.,.F.,(4,3,3,3,3,3,3,4),(-22.695939185231,
-21.9472133627188,-20.9496127553225,-19.9520121479262,-18.9544115405299,
-17.9568109331336,-16.9592103257373,-16.4127538780514),.UNSPECIFIED.);
#1180=B_SPLINE_CURVE_WITH_KNOTS('',3,(#8791,#8792,#8793,#8794,#8795,#8796,
#8797,#8798,#8799,#8800,#8801,#8802,#8803,#8804,#8805,#8806,#8807,#8808,
#8809,#8810,#8811,#8812,#8813,#8814,#8815),.UNSPECIFIED.,.F.,.F.,(4,3,3,
3,3,3,3,3,4),(13.8761928695311,13.9664085035483,14.9640091109446,15.9616097183409,
16.9592103257373,17.9568109331336,18.9544115405299,19.9520121479262,20.1593781767107),
 .UNSPECIFIED.);
#1181=B_SPLINE_CURVE_WITH_KNOTS('',3,(#8816,#8817,#8818,#8819,#8820,#8821,
#8822,#8823,#8824,#8825,#8826,#8827,#8828,#8829,#8830,#8831,#8832,#8833,
#8834,#8835,#8836,#8837),.UNSPECIFIED.,.F.,.F.,(4,3,3,3,3,3,3,4),(-16.4127538780514,
-15.9616097183409,-14.9640091109446,-13.9664085035483,-12.968807896152,
-11.9712072887557,-10.9736066813594,-10.1295685708718),.UNSPECIFIED.);
#1182=B_SPLINE_CURVE_WITH_KNOTS('',3,(#8843,#8844,#8845,#8846,#8847,#8848,
#8849,#8850,#8851,#8852,#8853,#8854,#8855),.UNSPECIFIED.,.F.,.F.,(4,3,3,
3,4),(-3.84638326369224,-2.99280182218893,-1.99520121479262,-0.99760060739631,
0.),.UNSPECIFIED.);
#1183=B_SPLINE_CURVE_WITH_KNOTS('',3,(#8858,#8859,#8860,#8861,#8862,#8863,
#8864,#8865,#8866,#8867,#8868,#8869,#8870,#8871,#8872,#8873,#8874,#8875,
#8876),.UNSPECIFIED.,.F.,.F.,(4,3,3,3,3,3,4),(2.01461286527443,2.99280182218893,
3.99040242958524,4.98800303698155,5.98560364437786,6.98320425177416,7.59300756235153),
 .UNSPECIFIED.);
#1184=B_SPLINE_CURVE_WITH_KNOTS('',3,(#8882,#8883,#8884,#8885,#8886,#8887,
#8888,#8889,#8890,#8891,#8892,#8893,#8894),.UNSPECIFIED.,.F.,.F.,(4,3,3,
3,4),(70.4248606341474,70.8296431251379,71.8272437325342,72.8248443399306,
73.8224449473269),.UNSPECIFIED.);
#1185=B_SPLINE_CURVE_WITH_KNOTS('',3,(#8897,#8898,#8899,#8900,#8901,#8902,
#8903,#8904,#8905,#8906,#8907,#8908,#8909,#8910,#8911,#8912,#8913,#8914,
#8915),.UNSPECIFIED.,.F.,.F.,(4,3,3,3,3,3,4),(-71.8078320820524,-70.829643125138,
-69.8320425177416,-68.8344419103453,-67.836841302949,-66.8392406955527,
-66.6782363354882),.UNSPECIFIED.);
#1186=B_SPLINE_CURVE_WITH_KNOTS('',3,(#8920,#8921,#8922,#8923,#8924,#8925,
#8926,#8927,#8928,#8929,#8930,#8931,#8932,#8933,#8934,#8935,#8936,#8937,
#8938,#8939,#8940,#8941),.UNSPECIFIED.,.F.,.F.,(4,3,3,3,3,3,3,4),(64.1416753269678,
64.8440394807601,65.8416400881564,66.8392406955527,67.836841302949,68.8344419103453,
69.8320425177416,70.4248606341474),.UNSPECIFIED.);
#1187=B_SPLINE_CURVE_WITH_KNOTS('',3,(#8942,#8943,#8944,#8945,#8946,#8947,
#8948,#8949,#8950,#8951,#8952,#8953,#8954,#8955,#8956,#8957,#8958,#8959,
#8960,#8961,#8962,#8963),.UNSPECIFIED.,.F.,.F.,(4,3,3,3,3,3,3,4),(-66.6782363354882,
-65.8416400881564,-64.8440394807601,-63.8464388733638,-62.8488382659675,
-61.8512376585712,-60.8536370511749,-60.3950510283086),.UNSPECIFIED.);
#1188=B_SPLINE_CURVE_WITH_KNOTS('',3,(#8968,#8969,#8970,#8971,#8972,#8973,
#8974,#8975,#8976,#8977,#8978,#8979,#8980,#8981,#8982,#8983,#8984,#8985,
#8986,#8987,#8988,#8989),.UNSPECIFIED.,.F.,.F.,(4,3,3,3,3,3,3,4),(57.8584900197882,
58.8584358363822,59.8560364437785,60.8536370511749,61.8512376585712,62.8488382659675,
63.8464388733638,64.1416753269678),.UNSPECIFIED.);
#1189=B_SPLINE_CURVE_WITH_KNOTS('',3,(#8990,#8991,#8992,#8993,#8994,#8995,
#8996,#8997,#8998,#8999,#9000,#9001,#9002,#9003,#9004,#9005,#9006,#9007,
#9008,#9009,#9010,#9011),.UNSPECIFIED.,.F.,.F.,(4,3,3,3,3,3,3,4),(-60.3950510283086,
-59.8560364437785,-58.8584358363822,-57.8608352289859,-56.8632346215896,
-55.8656340141933,-54.868033406797,-54.111865721129),.UNSPECIFIED.);
#1190=B_SPLINE_CURVE_WITH_KNOTS('',3,(#9016,#9017,#9018,#9019,#9020,#9021,
#9022,#9023,#9024,#9025,#9026,#9027,#9028,#9029,#9030,#9031,#9032,#9033,
#9034,#9035,#9036,#9037),.UNSPECIFIED.,.F.,.F.,(4,3,3,3,3,3,3,4),(51.5753047126087,
51.8752315846081,52.8728321920044,53.8704327994007,54.868033406797,55.8656340141933,
56.8632346215896,57.8584900197882),.UNSPECIFIED.);
#1191=B_SPLINE_CURVE_WITH_KNOTS('',3,(#9038,#9039,#9040,#9041,#9042,#9043,
#9044,#9045,#9046,#9047,#9048,#9049,#9050,#9051,#9052,#9053,#9054,#9055,
#9056,#9057,#9058,#9059,#9060,#9061,#9062),.UNSPECIFIED.,.F.,.F.,(4,3,3,
3,3,3,3,3,4),(-54.111865721129,-53.8704327994007,-52.8728321920044,-51.8752315846081,
-50.8776309772118,-49.8800303698155,-48.8824297624191,-47.8848291550228,
-47.8286804139494),.UNSPECIFIED.);
#1192=B_SPLINE_CURVE_WITH_KNOTS('',3,(#9067,#9068,#9069,#9070,#9071,#9072,
#9073,#9074,#9075,#9076,#9077,#9078,#9079,#9080,#9081,#9082,#9083,#9084,
#9085,#9086,#9087,#9088),.UNSPECIFIED.,.F.,.F.,(4,3,3,3,3,3,3,4),(45.2921194054291,
45.8896279402302,46.8872285476265,47.8848291550228,48.8824297624192,49.8800303698155,
50.8776309772118,51.5753047126087),.UNSPECIFIED.);
#1193=B_SPLINE_CURVE_WITH_KNOTS('',3,(#9089,#9090,#9091,#9092,#9093,#9094,
#9095,#9096,#9097,#9098,#9099,#9100,#9101,#9102,#9103,#9104,#9105,#9106,
#9107,#9108,#9109,#9110),.UNSPECIFIED.,.F.,.F.,(4,3,3,3,3,3,3,4),(-47.8286804139494,
-46.8872285476265,-45.8896279402302,-44.8920273328339,-43.8944267254376,
-42.8968261180413,-41.899225510645,-41.5454951067698),.UNSPECIFIED.);
#1194=B_SPLINE_CURVE_WITH_KNOTS('',3,(#9115,#9116,#9117,#9118,#9119,#9120,
#9121,#9122,#9123,#9124,#9125,#9126,#9127,#9128,#9129,#9130,#9131,#9132,
#9133,#9134,#9135,#9136),.UNSPECIFIED.,.F.,.F.,(4,3,3,3,3,3,3,4),(39.0089340982495,
39.9040242958524,40.9016249032487,41.899225510645,42.8968261180413,43.8944267254376,
44.8920273328339,45.2921194054291),.UNSPECIFIED.);
#1195=B_SPLINE_CURVE_WITH_KNOTS('',3,(#9137,#9138,#9139,#9140,#9141,#9142,
#9143,#9144,#9145,#9146,#9147,#9148,#9149,#9150,#9151,#9152,#9153,#9154,
#9155,#9156,#9157,#9158),.UNSPECIFIED.,.F.,.F.,(4,3,3,3,3,3,3,4),(-41.5454951067698,
-40.9016249032487,-39.9040242958524,-38.9064236884561,-37.9088230810597,
-36.9112224736634,-35.9136218662671,-35.2623097995902),.UNSPECIFIED.);
#1196=B_SPLINE_CURVE_WITH_KNOTS('',3,(#9163,#9164,#9165,#9166,#9167,#9168,
#9169,#9170,#9171,#9172,#9173,#9174,#9175,#9176,#9177,#9178,#9179,#9180,
#9181,#9182,#9183,#9184,#9185,#9186,#9187),.UNSPECIFIED.,.F.,.F.,(4,3,3,
3,3,3,3,3,4),(32.7257487910699,32.9208200440782,33.9184206514745,34.9160212588708,
35.9136218662671,36.9112224736634,37.9088230810598,38.9064236884561,39.0089340982495),
 .UNSPECIFIED.);
#1197=B_SPLINE_CURVE_WITH_KNOTS('',3,(#9188,#9189,#9190,#9191,#9192,#9193,
#9194,#9195,#9196,#9197,#9198,#9199,#9200,#9201,#9202,#9203,#9204,#9205,
#9206,#9207,#9208,#9209),.UNSPECIFIED.,.F.,.F.,(4,3,3,3,3,3,3,4),(-35.2623097995902,
-34.9160212588708,-33.9184206514745,-32.9208200440782,-31.9232194366819,
-30.9256188292856,-29.9280182218893,-28.9791244924106),.UNSPECIFIED.);
#1198=B_SPLINE_CURVE_WITH_KNOTS('',3,(#9214,#9215,#9216,#9217,#9218,#9219,
#9220,#9221,#9222,#9223,#9224,#9225,#9226,#9227,#9228,#9229,#9230,#9231,
#9232,#9233,#9234,#9235),.UNSPECIFIED.,.F.,.F.,(4,3,3,3,3,3,3,4),(26.4425634838903,
26.9352163997003,27.9328170070967,28.930417614493,29.9280182218893,30.9256188292856,
31.9232194366819,32.7257487910699),.UNSPECIFIED.);
#1199=B_SPLINE_CURVE_WITH_KNOTS('',3,(#9236,#9237,#9238,#9239,#9240,#9241,
#9242,#9243,#9244,#9245,#9246,#9247,#9248,#9249,#9250,#9251,#9252,#9253,
#9254,#9255,#9256,#9257,#9258,#9259,#9260),.UNSPECIFIED.,.F.,.F.,(4,3,3,
3,3,3,3,3,4),(-28.9791244924106,-28.930417614493,-27.9328170070967,-26.9352163997003,
-25.937615792304,-24.9400151849077,-23.9424145775114,-22.9448139701151,
-22.695939185231),.UNSPECIFIED.);
#1200=B_SPLINE_CURVE_WITH_KNOTS('',3,(#9265,#9266,#9267,#9268,#9269,#9270,
#9271,#9272,#9273,#9274,#9275,#9276,#9277,#9278,#9279,#9280,#9281,#9282,
#9283,#9284,#9285,#9286),.UNSPECIFIED.,.F.,.F.,(4,3,3,3,3,3,3,4),(20.1593781767107,
20.9496127553225,21.9472133627188,22.9448139701151,23.9424145775114,24.9400151849077,
25.937615792304,26.4425634838903),.UNSPECIFIED.);
#1201=B_SPLINE_CURVE_WITH_KNOTS('',3,(#9287,#9288,#9289,#9290,#9291,#9292,
#9293,#9294,#9295,#9296,#9297,#9298,#9299,#9300,#9301,#9302,#9303,#9304,
#9305,#9306,#9307,#9308),.UNSPECIFIED.,.F.,.F.,(4,3,3,3,3,3,3,4),(-22.695939185231,
-21.9472133627188,-20.9496127553225,-19.9520121479262,-18.9544115405299,
-17.9568109331336,-16.9592103257373,-16.4127538780514),.UNSPECIFIED.);
#1202=B_SPLINE_CURVE_WITH_KNOTS('',3,(#9313,#9314,#9315,#9316,#9317,#9318,
#9319,#9320,#9321,#9322,#9323,#9324,#9325,#9326,#9327,#9328,#9329,#9330,
#9331,#9332,#9333,#9334,#9335,#9336,#9337),.UNSPECIFIED.,.F.,.F.,(4,3,3,
3,3,3,3,3,4),(13.8761928695311,13.9664085035483,14.9640091109446,15.9616097183409,
16.9592103257373,17.9568109331336,18.9544115405299,19.9520121479262,20.1593781767107),
 .UNSPECIFIED.);
#1203=B_SPLINE_CURVE_WITH_KNOTS('',3,(#9338,#9339,#9340,#9341,#9342,#9343,
#9344,#9345,#9346,#9347,#9348,#9349,#9350,#9351,#9352,#9353,#9354,#9355,
#9356,#9357,#9358,#9359),.UNSPECIFIED.,.F.,.F.,(4,3,3,3,3,3,3,4),(-16.4127538780514,
-15.9616097183409,-14.9640091109446,-13.9664085035483,-12.968807896152,
-11.9712072887557,-10.9736066813594,-10.1295685708718),.UNSPECIFIED.);
#1204=B_SPLINE_CURVE_WITH_KNOTS('',3,(#9365,#9366,#9367,#9368,#9369,#9370,
#9371,#9372,#9373,#9374,#9375,#9376,#9377),.UNSPECIFIED.,.F.,.F.,(4,3,3,
3,4),(-3.84638326369225,-2.99280182218893,-1.99520121479262,-0.997600607396308,
0.),.UNSPECIFIED.);
#1205=B_SPLINE_CURVE_WITH_KNOTS('',3,(#9380,#9381,#9382,#9383,#9384,#9385,
#9386,#9387,#9388,#9389,#9390,#9391,#9392,#9393,#9394,#9395,#9396,#9397,
#9398),.UNSPECIFIED.,.F.,.F.,(4,3,3,3,3,3,4),(2.01461286527445,2.99280182218893,
3.99040242958524,4.98800303698155,5.98560364437786,6.98320425177416,7.59300756235153),
 .UNSPECIFIED.);
#1206=B_SPLINE_CURVE_WITH_KNOTS('',3,(#9404,#9405,#9406,#9407,#9408,#9409,
#9410,#9411,#9412,#9413,#9414,#9415,#9416),.UNSPECIFIED.,.F.,.F.,(4,3,3,
3,4),(70.4248606341474,70.8296431251379,71.8272437325342,72.8248443399306,
73.8224449473269),.UNSPECIFIED.);
#1207=B_SPLINE_CURVE_WITH_KNOTS('',3,(#9419,#9420,#9421,#9422,#9423,#9424,
#9425,#9426,#9427,#9428,#9429,#9430,#9431,#9432,#9433,#9434,#9435,#9436,
#9437),.UNSPECIFIED.,.F.,.F.,(4,3,3,3,3,3,4),(-71.8078320820524,-70.829643125138,
-69.8320425177417,-68.8344419103453,-67.836841302949,-66.8392406955527,
-66.6782363354881),.UNSPECIFIED.);
#1208=B_SPLINE_CURVE_WITH_KNOTS('',3,(#9442,#9443,#9444,#9445,#9446,#9447,
#9448,#9449,#9450,#9451,#9452,#9453,#9454,#9455,#9456,#9457,#9458,#9459,
#9460,#9461,#9462,#9463),.UNSPECIFIED.,.F.,.F.,(4,3,3,3,3,3,3,4),(64.1416753269678,
64.8440394807601,65.8416400881564,66.8392406955527,67.836841302949,68.8344419103453,
69.8320425177416,70.4248606341474),.UNSPECIFIED.);
#1209=B_SPLINE_CURVE_WITH_KNOTS('',3,(#9464,#9465,#9466,#9467,#9468,#9469,
#9470,#9471,#9472,#9473,#9474,#9475,#9476,#9477,#9478,#9479,#9480,#9481,
#9482,#9483,#9484,#9485),.UNSPECIFIED.,.F.,.F.,(4,3,3,3,3,3,3,4),(-66.6782363354881,
-65.8416400881564,-64.8440394807601,-63.8464388733638,-62.8488382659675,
-61.8512376585712,-60.8536370511749,-60.3950510283085),.UNSPECIFIED.);
#1210=B_SPLINE_CURVE_WITH_KNOTS('',3,(#9490,#9491,#9492,#9493,#9494,#9495,
#9496,#9497,#9498,#9499,#9500,#9501,#9502,#9503,#9504,#9505,#9506,#9507,
#9508,#9509,#9510,#9511),.UNSPECIFIED.,.F.,.F.,(4,3,3,3,3,3,3,4),(57.8584900197882,
58.8584358363823,59.8560364437786,60.8536370511749,61.8512376585712,62.8488382659675,
63.8464388733638,64.1416753269678),.UNSPECIFIED.);
#1211=B_SPLINE_CURVE_WITH_KNOTS('',3,(#9512,#9513,#9514,#9515,#9516,#9517,
#9518,#9519,#9520,#9521,#9522,#9523,#9524,#9525,#9526,#9527,#9528,#9529,
#9530,#9531,#9532,#9533),.UNSPECIFIED.,.F.,.F.,(4,3,3,3,3,3,3,4),(-60.3950510283085,
-59.8560364437786,-58.8584358363823,-57.8608352289859,-56.8632346215896,
-55.8656340141933,-54.868033406797,-54.111865721129),.UNSPECIFIED.);
#1212=B_SPLINE_CURVE_WITH_KNOTS('',3,(#9538,#9539,#9540,#9541,#9542,#9543,
#9544,#9545,#9546,#9547,#9548,#9549,#9550,#9551,#9552,#9553,#9554,#9555,
#9556,#9557,#9558,#9559),.UNSPECIFIED.,.F.,.F.,(4,3,3,3,3,3,3,4),(51.5753047126087,
51.8752315846081,52.8728321920044,53.8704327994007,54.868033406797,55.8656340141933,
56.8632346215896,57.8584900197882),.UNSPECIFIED.);
#1213=B_SPLINE_CURVE_WITH_KNOTS('',3,(#9560,#9561,#9562,#9563,#9564,#9565,
#9566,#9567,#9568,#9569,#9570,#9571,#9572,#9573,#9574,#9575,#9576,#9577,
#9578,#9579,#9580,#9581,#9582,#9583,#9584),.UNSPECIFIED.,.F.,.F.,(4,3,3,
3,3,3,3,3,4),(-54.111865721129,-53.8704327994007,-52.8728321920044,-51.8752315846081,
-50.8776309772118,-49.8800303698155,-48.8824297624192,-47.8848291550228,
-47.8286804139494),.UNSPECIFIED.);
#1214=B_SPLINE_CURVE_WITH_KNOTS('',3,(#9589,#9590,#9591,#9592,#9593,#9594,
#9595,#9596,#9597,#9598,#9599,#9600,#9601,#9602,#9603,#9604,#9605,#9606,
#9607,#9608,#9609,#9610),.UNSPECIFIED.,.F.,.F.,(4,3,3,3,3,3,3,4),(45.2921194054291,
45.8896279402302,46.8872285476265,47.8848291550228,48.8824297624192,49.8800303698155,
50.8776309772118,51.5753047126087),.UNSPECIFIED.);
#1215=B_SPLINE_CURVE_WITH_KNOTS('',3,(#9611,#9612,#9613,#9614,#9615,#9616,
#9617,#9618,#9619,#9620,#9621,#9622,#9623,#9624,#9625,#9626,#9627,#9628,
#9629,#9630,#9631,#9632),.UNSPECIFIED.,.F.,.F.,(4,3,3,3,3,3,3,4),(-47.8286804139494,
-46.8872285476265,-45.8896279402302,-44.8920273328339,-43.8944267254376,
-42.8968261180413,-41.899225510645,-41.5454951067698),.UNSPECIFIED.);
#1216=B_SPLINE_CURVE_WITH_KNOTS('',3,(#9637,#9638,#9639,#9640,#9641,#9642,
#9643,#9644,#9645,#9646,#9647,#9648,#9649,#9650,#9651,#9652,#9653,#9654,
#9655,#9656,#9657,#9658),.UNSPECIFIED.,.F.,.F.,(4,3,3,3,3,3,3,4),(39.0089340982495,
39.9040242958524,40.9016249032487,41.899225510645,42.8968261180413,43.8944267254376,
44.8920273328339,45.2921194054291),.UNSPECIFIED.);
#1217=B_SPLINE_CURVE_WITH_KNOTS('',3,(#9659,#9660,#9661,#9662,#9663,#9664,
#9665,#9666,#9667,#9668,#9669,#9670,#9671,#9672,#9673,#9674,#9675,#9676,
#9677,#9678,#9679,#9680),.UNSPECIFIED.,.F.,.F.,(4,3,3,3,3,3,3,4),(-41.5454951067698,
-40.9016249032487,-39.9040242958524,-38.9064236884561,-37.9088230810597,
-36.9112224736634,-35.9136218662671,-35.2623097995902),.UNSPECIFIED.);
#1218=B_SPLINE_CURVE_WITH_KNOTS('',3,(#9685,#9686,#9687,#9688,#9689,#9690,
#9691,#9692,#9693,#9694,#9695,#9696,#9697,#9698,#9699,#9700,#9701,#9702,
#9703,#9704,#9705,#9706,#9707,#9708,#9709),.UNSPECIFIED.,.F.,.F.,(4,3,3,
3,3,3,3,3,4),(32.7257487910699,32.9208200440782,33.9184206514745,34.9160212588708,
35.9136218662671,36.9112224736634,37.9088230810597,38.9064236884561,39.0089340982495),
 .UNSPECIFIED.);
#1219=B_SPLINE_CURVE_WITH_KNOTS('',3,(#9710,#9711,#9712,#9713,#9714,#9715,
#9716,#9717,#9718,#9719,#9720,#9721,#9722,#9723,#9724,#9725,#9726,#9727,
#9728,#9729,#9730,#9731),.UNSPECIFIED.,.F.,.F.,(4,3,3,3,3,3,3,4),(-35.2623097995902,
-34.9160212588708,-33.9184206514745,-32.9208200440782,-31.9232194366819,
-30.9256188292856,-29.9280182218893,-28.9791244924106),.UNSPECIFIED.);
#1220=B_SPLINE_CURVE_WITH_KNOTS('',3,(#9736,#9737,#9738,#9739,#9740,#9741,
#9742,#9743,#9744,#9745,#9746,#9747,#9748,#9749,#9750,#9751,#9752,#9753,
#9754,#9755,#9756,#9757),.UNSPECIFIED.,.F.,.F.,(4,3,3,3,3,3,3,4),(26.4425634838903,
26.9352163997003,27.9328170070966,28.930417614493,29.9280182218893,30.9256188292856,
31.9232194366819,32.7257487910699),.UNSPECIFIED.);
#1221=B_SPLINE_CURVE_WITH_KNOTS('',3,(#9758,#9759,#9760,#9761,#9762,#9763,
#9764,#9765,#9766,#9767,#9768,#9769,#9770,#9771,#9772,#9773,#9774,#9775,
#9776,#9777,#9778,#9779,#9780,#9781,#9782),.UNSPECIFIED.,.F.,.F.,(4,3,3,
3,3,3,3,3,4),(-28.9791244924106,-28.930417614493,-27.9328170070967,-26.9352163997004,
-25.937615792304,-24.9400151849077,-23.9424145775114,-22.9448139701151,
-22.695939185231),.UNSPECIFIED.);
#1222=B_SPLINE_CURVE_WITH_KNOTS('',3,(#9787,#9788,#9789,#9790,#9791,#9792,
#9793,#9794,#9795,#9796,#9797,#9798,#9799,#9800,#9801,#9802,#9803,#9804,
#9805,#9806,#9807,#9808),.UNSPECIFIED.,.F.,.F.,(4,3,3,3,3,3,3,4),(20.1593781767107,
20.9496127553225,21.9472133627188,22.9448139701151,23.9424145775114,24.9400151849077,
25.937615792304,26.4425634838903),.UNSPECIFIED.);
#1223=B_SPLINE_CURVE_WITH_KNOTS('',3,(#9809,#9810,#9811,#9812,#9813,#9814,
#9815,#9816,#9817,#9818,#9819,#9820,#9821,#9822,#9823,#9824,#9825,#9826,
#9827,#9828,#9829,#9830),.UNSPECIFIED.,.F.,.F.,(4,3,3,3,3,3,3,4),(-22.695939185231,
-21.9472133627188,-20.9496127553225,-19.9520121479262,-18.9544115405299,
-17.9568109331336,-16.9592103257373,-16.4127538780514),.UNSPECIFIED.);
#1224=B_SPLINE_CURVE_WITH_KNOTS('',3,(#9835,#9836,#9837,#9838,#9839,#9840,
#9841,#9842,#9843,#9844,#9845,#9846,#9847,#9848,#9849,#9850,#9851,#9852,
#9853,#9854,#9855,#9856,#9857,#9858,#9859),.UNSPECIFIED.,.F.,.F.,(4,3,3,
3,3,3,3,3,4),(13.8761928695311,13.9664085035483,14.9640091109446,15.9616097183409,
16.9592103257373,17.9568109331336,18.9544115405299,19.9520121479262,20.1593781767107),
 .UNSPECIFIED.);
#1225=B_SPLINE_CURVE_WITH_KNOTS('',3,(#9860,#9861,#9862,#9863,#9864,#9865,
#9866,#9867,#9868,#9869,#9870,#9871,#9872,#9873,#9874,#9875,#9876,#9877,
#9878,#9879,#9880,#9881),.UNSPECIFIED.,.F.,.F.,(4,3,3,3,3,3,3,4),(-16.4127538780514,
-15.9616097183409,-14.9640091109446,-13.9664085035483,-12.968807896152,
-11.9712072887557,-10.9736066813594,-10.1295685708718),.UNSPECIFIED.);
#1226=B_SPLINE_CURVE_WITH_KNOTS('',3,(#9887,#9888,#9889,#9890,#9891,#9892,
#9893,#9894,#9895,#9896,#9897,#9898,#9899),.UNSPECIFIED.,.F.,.F.,(4,3,3,
3,4),(-3.84638326369224,-2.99280182218893,-1.99520121479262,-0.99760060739631,
0.),.UNSPECIFIED.);
#1227=B_SPLINE_CURVE_WITH_KNOTS('',3,(#9904,#9905,#9906,#9907,#9908,#9909,
#9910,#9911,#9912,#9913,#9914,#9915,#9916,#9917,#9918,#9919,#9920,#9921,
#9922),.UNSPECIFIED.,.F.,.F.,(4,3,3,3,3,3,4),(2.01461286527445,2.99280182218893,
3.99040242958524,4.98800303698155,5.98560364437786,6.98320425177417,7.59300756235153),
 .UNSPECIFIED.);
#1228=B_SPLINE_CURVE_WITH_KNOTS('',3,(#9928,#9929,#9930,#9931,#9932,#9933,
#9934,#9935,#9936,#9937,#9938,#9939,#9940),.UNSPECIFIED.,.F.,.F.,(4,3,3,
3,4),(70.4248606341474,70.8296431251379,71.8272437325342,72.8248443399306,
73.8224449473269),.UNSPECIFIED.);
#1229=B_SPLINE_CURVE_WITH_KNOTS('',3,(#9943,#9944,#9945,#9946,#9947,#9948,
#9949,#9950,#9951,#9952,#9953,#9954,#9955,#9956,#9957,#9958,#9959,#9960,
#9961),.UNSPECIFIED.,.F.,.F.,(4,3,3,3,3,3,4),(-71.8078320820524,-70.8296431251379,
-69.8320425177416,-68.8344419103453,-67.836841302949,-66.8392406955527,
-66.6782363354881),.UNSPECIFIED.);
#1230=B_SPLINE_CURVE_WITH_KNOTS('',3,(#9966,#9967,#9968,#9969,#9970,#9971,
#9972,#9973,#9974,#9975,#9976,#9977,#9978,#9979,#9980,#9981,#9982,#9983,
#9984,#9985,#9986,#9987),.UNSPECIFIED.,.F.,.F.,(4,3,3,3,3,3,3,4),(64.1416753269678,
64.8440394807601,65.8416400881564,66.8392406955527,67.836841302949,68.8344419103453,
69.8320425177416,70.4248606341474),.UNSPECIFIED.);
#1231=B_SPLINE_CURVE_WITH_KNOTS('',3,(#9988,#9989,#9990,#9991,#9992,#9993,
#9994,#9995,#9996,#9997,#9998,#9999,#10000,#10001,#10002,#10003,#10004,
#10005,#10006,#10007,#10008,#10009),.UNSPECIFIED.,.F.,.F.,(4,3,3,3,3,3,
3,4),(-66.6782363354881,-65.8416400881564,-64.8440394807601,-63.8464388733638,
-62.8488382659675,-61.8512376585712,-60.8536370511749,-60.3950510283085),
 .UNSPECIFIED.);
#1232=B_SPLINE_CURVE_WITH_KNOTS('',3,(#10014,#10015,#10016,#10017,#10018,
#10019,#10020,#10021,#10022,#10023,#10024,#10025,#10026,#10027,#10028,#10029,
#10030,#10031,#10032,#10033,#10034,#10035),.UNSPECIFIED.,.F.,.F.,(4,3,3,
3,3,3,3,4),(57.8584900197882,58.8584358363823,59.8560364437786,60.8536370511749,
61.8512376585712,62.8488382659675,63.8464388733638,64.1416753269678),
 .UNSPECIFIED.);
#1233=B_SPLINE_CURVE_WITH_KNOTS('',3,(#10036,#10037,#10038,#10039,#10040,
#10041,#10042,#10043,#10044,#10045,#10046,#10047,#10048,#10049,#10050,#10051,
#10052,#10053,#10054,#10055,#10056,#10057),.UNSPECIFIED.,.F.,.F.,(4,3,3,
3,3,3,3,4),(-60.3950510283085,-59.8560364437785,-58.8584358363822,-57.8608352289859,
-56.8632346215896,-55.8656340141933,-54.868033406797,-54.111865721129),
 .UNSPECIFIED.);
#1234=B_SPLINE_CURVE_WITH_KNOTS('',3,(#10062,#10063,#10064,#10065,#10066,
#10067,#10068,#10069,#10070,#10071,#10072,#10073,#10074,#10075,#10076,#10077,
#10078,#10079,#10080,#10081,#10082,#10083),.UNSPECIFIED.,.F.,.F.,(4,3,3,
3,3,3,3,4),(51.5753047126087,51.8752315846081,52.8728321920044,53.8704327994007,
54.868033406797,55.8656340141933,56.8632346215896,57.8584900197882),
 .UNSPECIFIED.);
#1235=B_SPLINE_CURVE_WITH_KNOTS('',3,(#10084,#10085,#10086,#10087,#10088,
#10089,#10090,#10091,#10092,#10093,#10094,#10095,#10096,#10097,#10098,#10099,
#10100,#10101,#10102,#10103,#10104,#10105,#10106,#10107,#10108),
 .UNSPECIFIED.,.F.,.F.,(4,3,3,3,3,3,3,3,4),(-54.111865721129,-53.8704327994007,
-52.8728321920044,-51.8752315846081,-50.8776309772118,-49.8800303698155,
-48.8824297624191,-47.8848291550228,-47.8286804139494),.UNSPECIFIED.);
#1236=B_SPLINE_CURVE_WITH_KNOTS('',3,(#10113,#10114,#10115,#10116,#10117,
#10118,#10119,#10120,#10121,#10122,#10123,#10124,#10125,#10126,#10127,#10128,
#10129,#10130,#10131,#10132,#10133,#10134),.UNSPECIFIED.,.F.,.F.,(4,3,3,
3,3,3,3,4),(45.2921194054291,45.8896279402302,46.8872285476265,47.8848291550228,
48.8824297624192,49.8800303698155,50.8776309772118,51.5753047126087),
 .UNSPECIFIED.);
#1237=B_SPLINE_CURVE_WITH_KNOTS('',3,(#10135,#10136,#10137,#10138,#10139,
#10140,#10141,#10142,#10143,#10144,#10145,#10146,#10147,#10148,#10149,#10150,
#10151,#10152,#10153,#10154,#10155,#10156),.UNSPECIFIED.,.F.,.F.,(4,3,3,
3,3,3,3,4),(-47.8286804139494,-46.8872285476265,-45.8896279402302,-44.8920273328339,
-43.8944267254376,-42.8968261180413,-41.899225510645,-41.5454951067698),
 .UNSPECIFIED.);
#1238=B_SPLINE_CURVE_WITH_KNOTS('',3,(#10161,#10162,#10163,#10164,#10165,
#10166,#10167,#10168,#10169,#10170,#10171,#10172,#10173,#10174,#10175,#10176,
#10177,#10178,#10179,#10180,#10181,#10182),.UNSPECIFIED.,.F.,.F.,(4,3,3,
3,3,3,3,4),(39.0089340982495,39.9040242958524,40.9016249032487,41.899225510645,
42.8968261180413,43.8944267254376,44.8920273328339,45.2921194054291),
 .UNSPECIFIED.);
#1239=B_SPLINE_CURVE_WITH_KNOTS('',3,(#10183,#10184,#10185,#10186,#10187,
#10188,#10189,#10190,#10191,#10192,#10193,#10194,#10195,#10196,#10197,#10198,
#10199,#10200,#10201,#10202,#10203,#10204),.UNSPECIFIED.,.F.,.F.,(4,3,3,
3,3,3,3,4),(-41.5454951067698,-40.9016249032487,-39.9040242958524,-38.9064236884561,
-37.9088230810597,-36.9112224736634,-35.9136218662671,-35.2623097995902),
 .UNSPECIFIED.);
#1240=B_SPLINE_CURVE_WITH_KNOTS('',3,(#10209,#10210,#10211,#10212,#10213,
#10214,#10215,#10216,#10217,#10218,#10219,#10220,#10221,#10222,#10223,#10224,
#10225,#10226,#10227,#10228,#10229,#10230,#10231,#10232,#10233),
 .UNSPECIFIED.,.F.,.F.,(4,3,3,3,3,3,3,3,4),(32.7257487910699,32.9208200440782,
33.9184206514745,34.9160212588708,35.9136218662671,36.9112224736634,37.9088230810597,
38.9064236884561,39.0089340982495),.UNSPECIFIED.);
#1241=B_SPLINE_CURVE_WITH_KNOTS('',3,(#10234,#10235,#10236,#10237,#10238,
#10239,#10240,#10241,#10242,#10243,#10244,#10245,#10246,#10247,#10248,#10249,
#10250,#10251,#10252,#10253,#10254,#10255),.UNSPECIFIED.,.F.,.F.,(4,3,3,
3,3,3,3,4),(-35.2623097995902,-34.9160212588708,-33.9184206514745,-32.9208200440782,
-31.9232194366819,-30.9256188292856,-29.9280182218893,-28.9791244924106),
 .UNSPECIFIED.);
#1242=B_SPLINE_CURVE_WITH_KNOTS('',3,(#10260,#10261,#10262,#10263,#10264,
#10265,#10266,#10267,#10268,#10269,#10270,#10271,#10272,#10273,#10274,#10275,
#10276,#10277,#10278,#10279,#10280,#10281),.UNSPECIFIED.,.F.,.F.,(4,3,3,
3,3,3,3,4),(26.4425634838903,26.9352163997003,27.9328170070967,28.930417614493,
29.9280182218893,30.9256188292856,31.9232194366819,32.7257487910699),
 .UNSPECIFIED.);
#1243=B_SPLINE_CURVE_WITH_KNOTS('',3,(#10282,#10283,#10284,#10285,#10286,
#10287,#10288,#10289,#10290,#10291,#10292,#10293,#10294,#10295,#10296,#10297,
#10298,#10299,#10300,#10301,#10302,#10303,#10304,#10305,#10306),
 .UNSPECIFIED.,.F.,.F.,(4,3,3,3,3,3,3,3,4),(-28.9791244924106,-28.930417614493,
-27.9328170070967,-26.9352163997003,-25.937615792304,-24.9400151849077,
-23.9424145775114,-22.9448139701151,-22.695939185231),.UNSPECIFIED.);
#1244=B_SPLINE_CURVE_WITH_KNOTS('',3,(#10311,#10312,#10313,#10314,#10315,
#10316,#10317,#10318,#10319,#10320,#10321,#10322,#10323,#10324,#10325,#10326,
#10327,#10328,#10329,#10330,#10331,#10332),.UNSPECIFIED.,.F.,.F.,(4,3,3,
3,3,3,3,4),(20.1593781767107,20.9496127553225,21.9472133627188,22.9448139701151,
23.9424145775114,24.9400151849077,25.937615792304,26.4425634838903),
 .UNSPECIFIED.);
#1245=B_SPLINE_CURVE_WITH_KNOTS('',3,(#10333,#10334,#10335,#10336,#10337,
#10338,#10339,#10340,#10341,#10342,#10343,#10344,#10345,#10346,#10347,#10348,
#10349,#10350,#10351,#10352,#10353,#10354),.UNSPECIFIED.,.F.,.F.,(4,3,3,
3,3,3,3,4),(-22.695939185231,-21.9472133627188,-20.9496127553225,-19.9520121479262,
-18.9544115405299,-17.9568109331336,-16.9592103257372,-16.4127538780514),
 .UNSPECIFIED.);
#1246=B_SPLINE_CURVE_WITH_KNOTS('',3,(#10359,#10360,#10361,#10362,#10363,
#10364,#10365,#10366,#10367,#10368,#10369,#10370,#10371,#10372,#10373,#10374,
#10375,#10376,#10377,#10378,#10379,#10380,#10381,#10382,#10383),
 .UNSPECIFIED.,.F.,.F.,(4,3,3,3,3,3,3,3,4),(13.8761928695311,13.9664085035483,
14.9640091109446,15.9616097183409,16.9592103257373,17.9568109331336,18.9544115405299,
19.9520121479262,20.1593781767107),.UNSPECIFIED.);
#1247=B_SPLINE_CURVE_WITH_KNOTS('',3,(#10384,#10385,#10386,#10387,#10388,
#10389,#10390,#10391,#10392,#10393,#10394,#10395,#10396,#10397,#10398,#10399,
#10400,#10401,#10402,#10403,#10404,#10405),.UNSPECIFIED.,.F.,.F.,(4,3,3,
3,3,3,3,4),(-16.4127538780514,-15.9616097183409,-14.9640091109446,-13.9664085035483,
-12.968807896152,-11.9712072887557,-10.9736066813594,-10.1295685708718),
 .UNSPECIFIED.);
#1248=B_SPLINE_CURVE_WITH_KNOTS('',3,(#10411,#10412,#10413,#10414,#10415,
#10416,#10417,#10418,#10419,#10420,#10421,#10422,#10423),.UNSPECIFIED.,
 .F.,.F.,(4,3,3,3,4),(-3.84638326369224,-2.99280182218893,-1.99520121479262,
-0.99760060739631,0.),.UNSPECIFIED.);
#1249=B_SPLINE_CURVE_WITH_KNOTS('',3,(#10428,#10429,#10430,#10431,#10432,
#10433,#10434,#10435,#10436,#10437,#10438,#10439,#10440,#10441,#10442,#10443,
#10444,#10445,#10446),.UNSPECIFIED.,.F.,.F.,(4,3,3,3,3,3,4),(2.01461286527445,
2.99280182218893,3.99040242958524,4.98800303698155,5.98560364437786,6.98320425177417,
7.59300756235153),.UNSPECIFIED.);
#1250=B_SPLINE_CURVE_WITH_KNOTS('',3,(#10452,#10453,#10454,#10455),
 .UNSPECIFIED.,.F.,.F.,(4,4),(84.8230016469244,85.6840249515836),
 .UNSPECIFIED.);
#1251=B_SPLINE_CURVE_WITH_KNOTS('',3,(#10458,#10459,#10460,#10461,#10462),
 .UNSPECIFIED.,.F.,.F.,(4,1,4),(84.8230016469244,85.2277841379149,86.2059730948294),
 .UNSPECIFIED.);
#1252=B_SPLINE_CURVE_WITH_KNOTS('',3,(#10467,#10468,#10469,#10470,#10471,
#10472,#10473,#10474,#10475,#10476,#10477),.UNSPECIFIED.,.F.,.F.,(4,1,1,
1,1,1,1,1,4),(78.5398163397448,78.7008206998094,79.6984213072057,80.696021914602,
81.6936225219983,82.6912231293946,83.688823736791,84.6864243441873,84.8230016469244),
 .UNSPECIFIED.);
#1253=B_SPLINE_CURVE_WITH_KNOTS('',3,(#10478,#10479,#10480,#10481,#10482,
#10483,#10484,#10485,#10486,#10487),.UNSPECIFIED.,.F.,.F.,(4,1,1,1,1,1,
1,4),(78.5398163397448,79.242180493537,80.2397811009333,81.2373817083296,
82.2349823157259,83.2325829231223,84.2301835305186,84.8230016469244),
 .UNSPECIFIED.);
#1254=B_SPLINE_CURVE_WITH_KNOTS('',3,(#10492,#10493,#10494,#10495,#10496,
#10497,#10498,#10499,#10500,#10501),.UNSPECIFIED.,.F.,.F.,(4,1,1,1,1,1,
1,4),(72.2566310325652,72.7152170554315,73.7128176628279,74.7104182702242,
75.7080188776205,76.7056194850168,77.7032200924131,78.5398163397448),
 .UNSPECIFIED.);
#1255=B_SPLINE_CURVE_WITH_KNOTS('',3,(#10502,#10503,#10504,#10505,#10506,
#10507,#10508,#10509,#10510,#10511,#10512),.UNSPECIFIED.,.F.,.F.,(4,1,1,
1,1,1,1,1,4),(72.2566310325652,72.2589762417629,73.2565768491592,74.2541774565555,
75.2517780639518,76.2493786713481,77.2469792787444,78.2445798861407,78.5398163397448),
 .UNSPECIFIED.);
#1256=B_SPLINE_CURVE_WITH_KNOTS('',3,(#10517,#10518,#10519,#10520,#10521,
#10522,#10523,#10524,#10525,#10526),.UNSPECIFIED.,.F.,.F.,(4,1,1,1,1,1,
1,4),(65.9734457253856,66.7296134110537,67.72721401845,68.7248146258463,
69.7224152332426,70.7200158406389,71.7176164480352,72.2566310325652),
 .UNSPECIFIED.);
#1257=B_SPLINE_CURVE_WITH_KNOTS('',3,(#10527,#10528,#10529,#10530,#10531,
#10532,#10533,#10534,#10535,#10536),.UNSPECIFIED.,.F.,.F.,(4,1,1,1,1,1,
1,4),(65.9734457253856,66.273372597385,67.2709732047813,68.2685738121776,
69.2661744195739,70.2637750269702,71.2613756343666,72.2566310325652),
 .UNSPECIFIED.);
#1258=B_SPLINE_CURVE_WITH_KNOTS('',3,(#10541,#10542,#10543,#10544,#10545,
#10546,#10547,#10548,#10549,#10550,#10551),.UNSPECIFIED.,.F.,.F.,(4,1,1,
1,1,1,1,1,4),(59.690260418206,59.7464091592795,60.7440097666758,61.7416103740721,
62.7392109814685,63.7368115888648,64.7344121962611,65.7320128036574,65.9734457253856),
 .UNSPECIFIED.);
#1259=B_SPLINE_CURVE_WITH_KNOTS('',3,(#10552,#10553,#10554,#10555,#10556,
#10557,#10558,#10559,#10560,#10561),.UNSPECIFIED.,.F.,.F.,(4,1,1,1,1,1,
1,4),(59.6902604182061,60.2877689530072,61.2853695604035,62.2829701677998,
63.2805707751961,64.2781713825924,65.2757719899887,65.9734457253856),
 .UNSPECIFIED.);
#1260=B_SPLINE_CURVE_WITH_KNOTS('',3,(#10566,#10567,#10568,#10569,#10570,
#10571,#10572,#10573,#10574,#10575),.UNSPECIFIED.,.F.,.F.,(4,1,1,1,1,1,
1,4),(53.4070751110265,53.7608055149017,54.758406122298,55.7560067296943,
56.7536073370906,57.7512079444869,58.7488085518832,59.690260418206),
 .UNSPECIFIED.);
#1261=B_SPLINE_CURVE_WITH_KNOTS('',3,(#10576,#10577,#10578,#10579,#10580,
#10581,#10582,#10583,#10584,#10585),.UNSPECIFIED.,.F.,.F.,(4,1,1,1,1,1,
1,4),(53.4070751110265,54.3021653086293,55.2997659160256,56.2973665234219,
57.2949671308182,58.2925677382145,59.2901683456108,59.6902604182061),
 .UNSPECIFIED.);
#1262=B_SPLINE_CURVE_WITH_KNOTS('',3,(#10590,#10591,#10592,#10593,#10594,
#10595,#10596,#10597,#10598,#10599),.UNSPECIFIED.,.F.,.F.,(4,1,1,1,1,1,
1,4),(47.1238898038469,47.7752018705238,48.7728024779201,49.7704030853164,
50.7680036927127,51.7656043001091,52.7632049075054,53.4070751110265),
 .UNSPECIFIED.);
#1263=B_SPLINE_CURVE_WITH_KNOTS('',3,(#10600,#10601,#10602,#10603,#10604,
#10605,#10606,#10607,#10608,#10609,#10610),.UNSPECIFIED.,.F.,.F.,(4,1,1,
1,1,1,1,1,4),(47.1238898038469,47.3189610568551,48.3165616642514,49.3141622716478,
50.3117628790441,51.3093634864404,52.3069640938367,53.304564701233,53.4070751110265),
 .UNSPECIFIED.);
#1264=B_SPLINE_CURVE_WITH_KNOTS('',3,(#10615,#10616,#10617,#10618,#10619,
#10620,#10621,#10622,#10623,#10624),.UNSPECIFIED.,.F.,.F.,(4,1,1,1,1,1,
1,4),(40.8407044966673,41.789598226146,42.7871988335423,43.7847994409386,
44.7824000483349,45.7800006557312,46.7776012631275,47.1238898038469),
 .UNSPECIFIED.);
#1265=B_SPLINE_CURVE_WITH_KNOTS('',3,(#10625,#10626,#10627,#10628,#10629,
#10630,#10631,#10632,#10633,#10634),.UNSPECIFIED.,.F.,.F.,(4,1,1,1,1,1,
1,4),(40.8407044966673,41.3333574124773,42.3309580198736,43.3285586272699,
44.3261592346662,45.3237598420625,46.3213604494588,47.1238898038469),
 .UNSPECIFIED.);
#1266=B_SPLINE_CURVE_WITH_KNOTS('',3,(#10639,#10640,#10641,#10642,#10643,
#10644,#10645,#10646,#10647,#10648,#10649),.UNSPECIFIED.,.F.,.F.,(4,1,1,
1,1,1,1,1,4),(34.5575191894877,34.8063939743718,35.8039945817681,36.8015951891644,
37.7991957965607,38.796796403957,39.7943970113533,40.7919976187497,40.8407044966673),
 .UNSPECIFIED.);
#1267=B_SPLINE_CURVE_WITH_KNOTS('',3,(#10650,#10651,#10652,#10653,#10654,
#10655,#10656,#10657,#10658,#10659),.UNSPECIFIED.,.F.,.F.,(4,1,1,1,1,1,
1,4),(34.5575191894877,35.3477537680994,36.3453543754957,37.342954982892,
38.3405555902884,39.3381561976847,40.335756805081,40.8407044966673),
 .UNSPECIFIED.);
#1268=B_SPLINE_CURVE_WITH_KNOTS('',3,(#10664,#10665,#10666,#10667,#10668,
#10669,#10670,#10671,#10672,#10673),.UNSPECIFIED.,.F.,.F.,(4,1,1,1,1,1,
1,4),(28.2743338823081,28.8207903299939,29.8183909373903,30.8159915447866,
31.8135921521829,32.8111927595792,33.8087933669755,34.5575191894877),
 .UNSPECIFIED.);
#1269=B_SPLINE_CURVE_WITH_KNOTS('',3,(#10674,#10675,#10676,#10677,#10678,
#10679,#10680,#10681,#10682,#10683,#10684),.UNSPECIFIED.,.F.,.F.,(4,1,1,
1,1,1,1,1,4),(28.2743338823081,28.3645495163253,29.3621501237216,30.3597507311179,
31.3573513385142,32.3549519459105,33.3525525533068,34.3501531607031,34.5575191894877),
 .UNSPECIFIED.);
#1270=B_SPLINE_CURVE_WITH_KNOTS('',3,(#10689,#10690,#10691,#10692,#10693,
#10694,#10695,#10696,#10697,#10698),.UNSPECIFIED.,.F.,.F.,(4,1,1,1,1,1,
1,4),(21.9911485751285,22.8351866856161,23.8327872930124,24.8303879004087,
25.827988507805,26.8255891152013,27.8231897225976,28.2743338823081),
 .UNSPECIFIED.);
#1271=B_SPLINE_CURVE_WITH_KNOTS('',3,(#10699,#10700,#10701,#10702,#10703,
#10704,#10705,#10706,#10707,#10708),.UNSPECIFIED.,.F.,.F.,(4,1,1,1,1,1,
1,4),(21.9911485751285,22.3789458719474,23.3765464793437,24.37414708674,
25.3717476941363,26.3693483015326,27.366948908929,28.2743338823081),
 .UNSPECIFIED.);
#1272=B_SPLINE_CURVE_WITH_KNOTS('',3,(#10714,#10715,#10716,#10717,#10718),
 .UNSPECIFIED.,.F.,.F.,(4,1,4),(14.3981410127769,15.3957416201732,15.7079632679489),
 .UNSPECIFIED.);
#1273=B_SPLINE_CURVE_WITH_KNOTS('',3,(#10721,#10722,#10723,#10724,#10725),
 .UNSPECIFIED.,.F.,.F.,(4,1,4),(13.8761928695311,14.8543818264456,15.7079632679489),
 .UNSPECIFIED.);
#1274=B_SPLINE_CURVE_WITH_KNOTS('',3,(#10731,#10732,#10733,#10734),
 .UNSPECIFIED.,.F.,.F.,(4,4),(84.8230016469244,85.6840249515836),
 .UNSPECIFIED.);
#1275=B_SPLINE_CURVE_WITH_KNOTS('',3,(#10737,#10738,#10739,#10740,#10741),
 .UNSPECIFIED.,.F.,.F.,(4,1,4),(84.8230016469244,85.2277841379149,86.2059730948294),
 .UNSPECIFIED.);
#1276=B_SPLINE_CURVE_WITH_KNOTS('',3,(#10746,#10747,#10748,#10749,#10750,
#10751,#10752,#10753,#10754,#10755,#10756),.UNSPECIFIED.,.F.,.F.,(4,1,1,
1,1,1,1,1,4),(78.5398163397448,78.7008206998094,79.6984213072057,80.696021914602,
81.6936225219983,82.6912231293946,83.6888237367909,84.6864243441872,84.8230016469244),
 .UNSPECIFIED.);
#1277=B_SPLINE_CURVE_WITH_KNOTS('',3,(#10757,#10758,#10759,#10760,#10761,
#10762,#10763,#10764,#10765,#10766),.UNSPECIFIED.,.F.,.F.,(4,1,1,1,1,1,
1,4),(78.5398163397448,79.242180493537,80.2397811009333,81.2373817083296,
82.2349823157259,83.2325829231222,84.2301835305186,84.8230016469244),
 .UNSPECIFIED.);
#1278=B_SPLINE_CURVE_WITH_KNOTS('',3,(#10771,#10772,#10773,#10774,#10775,
#10776,#10777,#10778,#10779,#10780),.UNSPECIFIED.,.F.,.F.,(4,1,1,1,1,1,
1,4),(72.2566310325652,72.7152170554315,73.7128176628278,74.7104182702242,
75.7080188776205,76.7056194850168,77.7032200924131,78.5398163397448),
 .UNSPECIFIED.);
#1279=B_SPLINE_CURVE_WITH_KNOTS('',3,(#10781,#10782,#10783,#10784,#10785,
#10786,#10787,#10788,#10789,#10790,#10791),.UNSPECIFIED.,.F.,.F.,(4,1,1,
1,1,1,1,1,4),(72.2566310325652,72.2589762417629,73.2565768491592,74.2541774565555,
75.2517780639518,76.2493786713481,77.2469792787444,78.2445798861407,78.5398163397448),
 .UNSPECIFIED.);
#1280=B_SPLINE_CURVE_WITH_KNOTS('',3,(#10796,#10797,#10798,#10799,#10800,
#10801,#10802,#10803,#10804,#10805),.UNSPECIFIED.,.F.,.F.,(4,1,1,1,1,1,
1,4),(65.9734457253856,66.7296134110537,67.72721401845,68.7248146258463,
69.7224152332426,70.7200158406389,71.7176164480352,72.2566310325652),
 .UNSPECIFIED.);
#1281=B_SPLINE_CURVE_WITH_KNOTS('',3,(#10806,#10807,#10808,#10809,#10810,
#10811,#10812,#10813,#10814,#10815),.UNSPECIFIED.,.F.,.F.,(4,1,1,1,1,1,
1,4),(65.9734457253856,66.273372597385,67.2709732047813,68.2685738121776,
69.2661744195739,70.2637750269702,71.2613756343665,72.2566310325652),
 .UNSPECIFIED.);
#1282=B_SPLINE_CURVE_WITH_KNOTS('',3,(#10820,#10821,#10822,#10823,#10824,
#10825,#10826,#10827,#10828,#10829,#10830),.UNSPECIFIED.,.F.,.F.,(4,1,1,
1,1,1,1,1,4),(59.690260418206,59.7464091592795,60.7440097666758,61.7416103740721,
62.7392109814684,63.7368115888648,64.7344121962611,65.7320128036574,65.9734457253856),
 .UNSPECIFIED.);
#1283=B_SPLINE_CURVE_WITH_KNOTS('',3,(#10831,#10832,#10833,#10834,#10835,
#10836,#10837,#10838,#10839,#10840),.UNSPECIFIED.,.F.,.F.,(4,1,1,1,1,1,
1,4),(59.6902604182061,60.2877689530071,61.2853695604035,62.2829701677998,
63.2805707751961,64.2781713825924,65.2757719899887,65.9734457253856),
 .UNSPECIFIED.);
#1284=B_SPLINE_CURVE_WITH_KNOTS('',3,(#10845,#10846,#10847,#10848,#10849,
#10850,#10851,#10852,#10853,#10854),.UNSPECIFIED.,.F.,.F.,(4,1,1,1,1,1,
1,4),(53.4070751110265,53.7608055149017,54.758406122298,55.7560067296943,
56.7536073370906,57.7512079444869,58.7488085518832,59.690260418206),
 .UNSPECIFIED.);
#1285=B_SPLINE_CURVE_WITH_KNOTS('',3,(#10855,#10856,#10857,#10858,#10859,
#10860,#10861,#10862,#10863,#10864),.UNSPECIFIED.,.F.,.F.,(4,1,1,1,1,1,
1,4),(53.4070751110265,54.3021653086293,55.2997659160256,56.2973665234219,
57.2949671308182,58.2925677382145,59.2901683456108,59.6902604182061),
 .UNSPECIFIED.);
#1286=B_SPLINE_CURVE_WITH_KNOTS('',3,(#10869,#10870,#10871,#10872,#10873,
#10874,#10875,#10876,#10877,#10878),.UNSPECIFIED.,.F.,.F.,(4,1,1,1,1,1,
1,4),(47.1238898038469,47.7752018705238,48.7728024779201,49.7704030853164,
50.7680036927127,51.765604300109,52.7632049075054,53.4070751110265),
 .UNSPECIFIED.);
#1287=B_SPLINE_CURVE_WITH_KNOTS('',3,(#10879,#10880,#10881,#10882,#10883,
#10884,#10885,#10886,#10887,#10888,#10889),.UNSPECIFIED.,.F.,.F.,(4,1,1,
1,1,1,1,1,4),(47.1238898038469,47.3189610568551,48.3165616642514,49.3141622716477,
50.3117628790441,51.3093634864404,52.3069640938367,53.304564701233,53.4070751110265),
 .UNSPECIFIED.);
#1288=B_SPLINE_CURVE_WITH_KNOTS('',3,(#10894,#10895,#10896,#10897,#10898,
#10899,#10900,#10901,#10902,#10903),.UNSPECIFIED.,.F.,.F.,(4,1,1,1,1,1,
1,4),(40.8407044966673,41.7895982261459,42.7871988335423,43.7847994409386,
44.7824000483349,45.7800006557312,46.7776012631275,47.1238898038469),
 .UNSPECIFIED.);
#1289=B_SPLINE_CURVE_WITH_KNOTS('',3,(#10904,#10905,#10906,#10907,#10908,
#10909,#10910,#10911,#10912,#10913),.UNSPECIFIED.,.F.,.F.,(4,1,1,1,1,1,
1,4),(40.8407044966673,41.3333574124773,42.3309580198736,43.3285586272699,
44.3261592346662,45.3237598420625,46.3213604494588,47.1238898038469),
 .UNSPECIFIED.);
#1290=B_SPLINE_CURVE_WITH_KNOTS('',3,(#10918,#10919,#10920,#10921,#10922,
#10923,#10924,#10925,#10926,#10927,#10928),.UNSPECIFIED.,.F.,.F.,(4,1,1,
1,1,1,1,1,4),(34.5575191894877,34.8063939743718,35.8039945817681,36.8015951891644,
37.7991957965607,38.796796403957,39.7943970113533,40.7919976187496,40.8407044966673),
 .UNSPECIFIED.);
#1291=B_SPLINE_CURVE_WITH_KNOTS('',3,(#10929,#10930,#10931,#10932,#10933,
#10934,#10935,#10936,#10937,#10938),.UNSPECIFIED.,.F.,.F.,(4,1,1,1,1,1,
1,4),(34.5575191894877,35.3477537680994,36.3453543754957,37.342954982892,
38.3405555902883,39.3381561976846,40.335756805081,40.8407044966673),
 .UNSPECIFIED.);
#1292=B_SPLINE_CURVE_WITH_KNOTS('',3,(#10943,#10944,#10945,#10946,#10947,
#10948,#10949,#10950,#10951,#10952),.UNSPECIFIED.,.F.,.F.,(4,1,1,1,1,1,
1,4),(28.2743338823081,28.8207903299939,29.8183909373902,30.8159915447865,
31.8135921521829,32.8111927595792,33.8087933669755,34.5575191894877),
 .UNSPECIFIED.);
#1293=B_SPLINE_CURVE_WITH_KNOTS('',3,(#10953,#10954,#10955,#10956,#10957,
#10958,#10959,#10960,#10961,#10962,#10963),.UNSPECIFIED.,.F.,.F.,(4,1,1,
1,1,1,1,1,4),(28.2743338823081,28.3645495163252,29.3621501237216,30.3597507311179,
31.3573513385142,32.3549519459105,33.3525525533068,34.3501531607031,34.5575191894877),
 .UNSPECIFIED.);
#1294=B_SPLINE_CURVE_WITH_KNOTS('',3,(#10968,#10969,#10970,#10971,#10972,
#10973,#10974,#10975,#10976,#10977),.UNSPECIFIED.,.F.,.F.,(4,1,1,1,1,1,
1,4),(21.9911485751285,22.8351866856161,23.8327872930124,24.8303879004087,
25.827988507805,26.8255891152013,27.8231897225976,28.2743338823081),
 .UNSPECIFIED.);
#1295=B_SPLINE_CURVE_WITH_KNOTS('',3,(#10978,#10979,#10980,#10981,#10982,
#10983,#10984,#10985,#10986,#10987),.UNSPECIFIED.,.F.,.F.,(4,1,1,1,1,1,
1,4),(21.9911485751285,22.3789458719474,23.3765464793437,24.37414708674,
25.3717476941363,26.3693483015326,27.3669489089289,28.2743338823081),
 .UNSPECIFIED.);
#1296=B_SPLINE_CURVE_WITH_KNOTS('',3,(#10993,#10994,#10995,#10996,#10997),
 .UNSPECIFIED.,.F.,.F.,(4,1,4),(14.3981410127769,15.3957416201732,15.7079632679489),
 .UNSPECIFIED.);
#1297=B_SPLINE_CURVE_WITH_KNOTS('',3,(#11000,#11001,#11002,#11003,#11004),
 .UNSPECIFIED.,.F.,.F.,(4,1,4),(13.8761928695311,14.8543818264456,15.7079632679489),
 .UNSPECIFIED.);
#1298=B_SPLINE_CURVE_WITH_KNOTS('',3,(#11010,#11011,#11012,#11013),
 .UNSPECIFIED.,.F.,.F.,(4,4),(84.8230016469244,85.6840249515836),
 .UNSPECIFIED.);
#1299=B_SPLINE_CURVE_WITH_KNOTS('',3,(#11016,#11017,#11018,#11019,#11020),
 .UNSPECIFIED.,.F.,.F.,(4,1,4),(84.8230016469244,85.2277841379149,86.2059730948294),
 .UNSPECIFIED.);
#1300=B_SPLINE_CURVE_WITH_KNOTS('',3,(#11025,#11026,#11027,#11028,#11029,
#11030,#11031,#11032,#11033,#11034,#11035),.UNSPECIFIED.,.F.,.F.,(4,1,1,
1,1,1,1,1,4),(78.5398163397448,78.7008206998094,79.6984213072057,80.696021914602,
81.6936225219983,82.6912231293946,83.6888237367909,84.6864243441872,84.8230016469244),
 .UNSPECIFIED.);
#1301=B_SPLINE_CURVE_WITH_KNOTS('',3,(#11036,#11037,#11038,#11039,#11040,
#11041,#11042,#11043,#11044,#11045),.UNSPECIFIED.,.F.,.F.,(4,1,1,1,1,1,
1,4),(78.5398163397448,79.242180493537,80.2397811009333,81.2373817083296,
82.2349823157259,83.2325829231222,84.2301835305186,84.8230016469244),
 .UNSPECIFIED.);
#1302=B_SPLINE_CURVE_WITH_KNOTS('',3,(#11050,#11051,#11052,#11053,#11054,
#11055,#11056,#11057,#11058,#11059),.UNSPECIFIED.,.F.,.F.,(4,1,1,1,1,1,
1,4),(72.2566310325652,72.7152170554315,73.7128176628278,74.7104182702242,
75.7080188776205,76.7056194850168,77.7032200924131,78.5398163397448),
 .UNSPECIFIED.);
#1303=B_SPLINE_CURVE_WITH_KNOTS('',3,(#11060,#11061,#11062,#11063,#11064,
#11065,#11066,#11067,#11068,#11069,#11070),.UNSPECIFIED.,.F.,.F.,(4,1,1,
1,1,1,1,1,4),(72.2566310325652,72.2589762417629,73.2565768491592,74.2541774565555,
75.2517780639518,76.2493786713481,77.2469792787444,78.2445798861407,78.5398163397448),
 .UNSPECIFIED.);
#1304=B_SPLINE_CURVE_WITH_KNOTS('',3,(#11075,#11076,#11077,#11078,#11079,
#11080,#11081,#11082,#11083,#11084),.UNSPECIFIED.,.F.,.F.,(4,1,1,1,1,1,
1,4),(65.9734457253856,66.7296134110537,67.72721401845,68.7248146258463,
69.7224152332426,70.7200158406389,71.7176164480352,72.2566310325652),
 .UNSPECIFIED.);
#1305=B_SPLINE_CURVE_WITH_KNOTS('',3,(#11085,#11086,#11087,#11088,#11089,
#11090,#11091,#11092,#11093,#11094),.UNSPECIFIED.,.F.,.F.,(4,1,1,1,1,1,
1,4),(65.9734457253856,66.273372597385,67.2709732047813,68.2685738121776,
69.2661744195739,70.2637750269702,71.2613756343665,72.2566310325652),
 .UNSPECIFIED.);
#1306=B_SPLINE_CURVE_WITH_KNOTS('',3,(#11099,#11100,#11101,#11102,#11103,
#11104,#11105,#11106,#11107,#11108,#11109),.UNSPECIFIED.,.F.,.F.,(4,1,1,
1,1,1,1,1,4),(59.690260418206,59.7464091592795,60.7440097666758,61.7416103740721,
62.7392109814684,63.7368115888648,64.7344121962611,65.7320128036574,65.9734457253856),
 .UNSPECIFIED.);
#1307=B_SPLINE_CURVE_WITH_KNOTS('',3,(#11110,#11111,#11112,#11113,#11114,
#11115,#11116,#11117,#11118,#11119),.UNSPECIFIED.,.F.,.F.,(4,1,1,1,1,1,
1,4),(59.690260418206,60.2877689530071,61.2853695604035,62.2829701677998,
63.2805707751961,64.2781713825924,65.2757719899887,65.9734457253856),
 .UNSPECIFIED.);
#1308=B_SPLINE_CURVE_WITH_KNOTS('',3,(#11124,#11125,#11126,#11127,#11128,
#11129,#11130,#11131,#11132,#11133),.UNSPECIFIED.,.F.,.F.,(4,1,1,1,1,1,
1,4),(53.4070751110265,53.7608055149017,54.758406122298,55.7560067296943,
56.7536073370906,57.7512079444869,58.7488085518832,59.690260418206),
 .UNSPECIFIED.);
#1309=B_SPLINE_CURVE_WITH_KNOTS('',3,(#11134,#11135,#11136,#11137,#11138,
#11139,#11140,#11141,#11142,#11143),.UNSPECIFIED.,.F.,.F.,(4,1,1,1,1,1,
1,4),(53.4070751110265,54.3021653086293,55.2997659160256,56.2973665234219,
57.2949671308182,58.2925677382145,59.2901683456108,59.690260418206),
 .UNSPECIFIED.);
#1310=B_SPLINE_CURVE_WITH_KNOTS('',3,(#11148,#11149,#11150,#11151,#11152,
#11153,#11154,#11155,#11156,#11157),.UNSPECIFIED.,.F.,.F.,(4,1,1,1,1,1,
1,4),(47.1238898038469,47.7752018705238,48.7728024779201,49.7704030853164,
50.7680036927127,51.765604300109,52.7632049075054,53.4070751110265),
 .UNSPECIFIED.);
#1311=B_SPLINE_CURVE_WITH_KNOTS('',3,(#11158,#11159,#11160,#11161,#11162,
#11163,#11164,#11165,#11166,#11167,#11168),.UNSPECIFIED.,.F.,.F.,(4,1,1,
1,1,1,1,1,4),(47.1238898038469,47.3189610568551,48.3165616642514,49.3141622716477,
50.3117628790441,51.3093634864404,52.3069640938367,53.304564701233,53.4070751110265),
 .UNSPECIFIED.);
#1312=B_SPLINE_CURVE_WITH_KNOTS('',3,(#11173,#11174,#11175,#11176,#11177,
#11178,#11179,#11180,#11181,#11182),.UNSPECIFIED.,.F.,.F.,(4,1,1,1,1,1,
1,4),(40.8407044966673,41.7895982261459,42.7871988335423,43.7847994409386,
44.7824000483349,45.7800006557312,46.7776012631275,47.1238898038469),
 .UNSPECIFIED.);
#1313=B_SPLINE_CURVE_WITH_KNOTS('',3,(#11183,#11184,#11185,#11186,#11187,
#11188,#11189,#11190,#11191,#11192),.UNSPECIFIED.,.F.,.F.,(4,1,1,1,1,1,
1,4),(40.8407044966673,41.3333574124773,42.3309580198736,43.3285586272699,
44.3261592346662,45.3237598420625,46.3213604494588,47.1238898038469),
 .UNSPECIFIED.);
#1314=B_SPLINE_CURVE_WITH_KNOTS('',3,(#11197,#11198,#11199,#11200,#11201,
#11202,#11203,#11204,#11205,#11206,#11207),.UNSPECIFIED.,.F.,.F.,(4,1,1,
1,1,1,1,1,4),(34.5575191894877,34.8063939743718,35.8039945817681,36.8015951891644,
37.7991957965607,38.796796403957,39.7943970113533,40.7919976187496,40.8407044966673),
 .UNSPECIFIED.);
#1315=B_SPLINE_CURVE_WITH_KNOTS('',3,(#11208,#11209,#11210,#11211,#11212,
#11213,#11214,#11215,#11216,#11217),.UNSPECIFIED.,.F.,.F.,(4,1,1,1,1,1,
1,4),(34.5575191894877,35.3477537680994,36.3453543754957,37.342954982892,
38.3405555902883,39.3381561976846,40.335756805081,40.8407044966673),
 .UNSPECIFIED.);
#1316=B_SPLINE_CURVE_WITH_KNOTS('',3,(#11222,#11223,#11224,#11225,#11226,
#11227,#11228,#11229,#11230,#11231),.UNSPECIFIED.,.F.,.F.,(4,1,1,1,1,1,
1,4),(28.2743338823081,28.8207903299939,29.8183909373902,30.8159915447865,
31.8135921521829,32.8111927595792,33.8087933669755,34.5575191894877),
 .UNSPECIFIED.);
#1317=B_SPLINE_CURVE_WITH_KNOTS('',3,(#11232,#11233,#11234,#11235,#11236,
#11237,#11238,#11239,#11240,#11241,#11242),.UNSPECIFIED.,.F.,.F.,(4,1,1,
1,1,1,1,1,4),(28.2743338823081,28.3645495163252,29.3621501237216,30.3597507311179,
31.3573513385142,32.3549519459105,33.3525525533068,34.3501531607031,34.5575191894877),
 .UNSPECIFIED.);
#1318=B_SPLINE_CURVE_WITH_KNOTS('',3,(#11247,#11248,#11249,#11250,#11251,
#11252,#11253,#11254,#11255,#11256),.UNSPECIFIED.,.F.,.F.,(4,1,1,1,1,1,
1,4),(21.9911485751285,22.8351866856161,23.8327872930124,24.8303879004087,
25.827988507805,26.8255891152013,27.8231897225976,28.2743338823081),
 .UNSPECIFIED.);
#1319=B_SPLINE_CURVE_WITH_KNOTS('',3,(#11257,#11258,#11259,#11260,#11261,
#11262,#11263,#11264,#11265,#11266),.UNSPECIFIED.,.F.,.F.,(4,1,1,1,1,1,
1,4),(21.9911485751285,22.3789458719474,23.3765464793437,24.37414708674,
25.3717476941363,26.3693483015326,27.3669489089289,28.2743338823081),
 .UNSPECIFIED.);
#1320=B_SPLINE_CURVE_WITH_KNOTS('',3,(#11272,#11273,#11274,#11275,#11276),
 .UNSPECIFIED.,.F.,.F.,(4,1,4),(14.3981410127769,15.3957416201732,15.7079632679489),
 .UNSPECIFIED.);
#1321=B_SPLINE_CURVE_WITH_KNOTS('',3,(#11279,#11280,#11281,#11282,#11283),
 .UNSPECIFIED.,.F.,.F.,(4,1,4),(13.8761928695311,14.8543818264456,15.7079632679489),
 .UNSPECIFIED.);
#1322=B_SPLINE_CURVE_WITH_KNOTS('',3,(#11289,#11290,#11291,#11292),
 .UNSPECIFIED.,.F.,.F.,(4,4),(84.8230016469244,85.6840249515836),
 .UNSPECIFIED.);
#1323=B_SPLINE_CURVE_WITH_KNOTS('',3,(#11295,#11296,#11297,#11298,#11299),
 .UNSPECIFIED.,.F.,.F.,(4,1,4),(84.8230016469244,85.2277841379149,86.2059730948294),
 .UNSPECIFIED.);
#1324=B_SPLINE_CURVE_WITH_KNOTS('',3,(#11304,#11305,#11306,#11307,#11308,
#11309,#11310,#11311,#11312,#11313,#11314),.UNSPECIFIED.,.F.,.F.,(4,1,1,
1,1,1,1,1,4),(78.5398163397448,78.7008206998094,79.6984213072057,80.696021914602,
81.6936225219983,82.6912231293946,83.688823736791,84.6864243441873,84.8230016469244),
 .UNSPECIFIED.);
#1325=B_SPLINE_CURVE_WITH_KNOTS('',3,(#11315,#11316,#11317,#11318,#11319,
#11320,#11321,#11322,#11323,#11324),.UNSPECIFIED.,.F.,.F.,(4,1,1,1,1,1,
1,4),(78.5398163397448,79.242180493537,80.2397811009333,81.2373817083296,
82.2349823157259,83.2325829231223,84.2301835305186,84.8230016469244),
 .UNSPECIFIED.);
#1326=B_SPLINE_CURVE_WITH_KNOTS('',3,(#11329,#11330,#11331,#11332,#11333,
#11334,#11335,#11336,#11337,#11338),.UNSPECIFIED.,.F.,.F.,(4,1,1,1,1,1,
1,4),(72.2566310325652,72.7152170554316,73.7128176628279,74.7104182702242,
75.7080188776205,76.7056194850168,77.7032200924131,78.5398163397448),
 .UNSPECIFIED.);
#1327=B_SPLINE_CURVE_WITH_KNOTS('',3,(#11339,#11340,#11341,#11342,#11343,
#11344,#11345,#11346,#11347,#11348,#11349),.UNSPECIFIED.,.F.,.F.,(4,1,1,
1,1,1,1,1,4),(72.2566310325652,72.2589762417629,73.2565768491592,74.2541774565555,
75.2517780639518,76.2493786713481,77.2469792787444,78.2445798861407,78.5398163397448),
 .UNSPECIFIED.);
#1328=B_SPLINE_CURVE_WITH_KNOTS('',3,(#11354,#11355,#11356,#11357,#11358,
#11359,#11360,#11361,#11362,#11363),.UNSPECIFIED.,.F.,.F.,(4,1,1,1,1,1,
1,4),(65.9734457253856,66.7296134110537,67.72721401845,68.7248146258463,
69.7224152332426,70.7200158406389,71.7176164480352,72.2566310325652),
 .UNSPECIFIED.);
#1329=B_SPLINE_CURVE_WITH_KNOTS('',3,(#11364,#11365,#11366,#11367,#11368,
#11369,#11370,#11371,#11372,#11373),.UNSPECIFIED.,.F.,.F.,(4,1,1,1,1,1,
1,4),(65.9734457253856,66.273372597385,67.2709732047813,68.2685738121776,
69.2661744195739,70.2637750269702,71.2613756343666,72.2566310325652),
 .UNSPECIFIED.);
#1330=B_SPLINE_CURVE_WITH_KNOTS('',3,(#11378,#11379,#11380,#11381,#11382,
#11383,#11384,#11385,#11386,#11387,#11388),.UNSPECIFIED.,.F.,.F.,(4,1,1,
1,1,1,1,1,4),(59.690260418206,59.7464091592795,60.7440097666758,61.7416103740722,
62.7392109814685,63.7368115888648,64.7344121962611,65.7320128036574,65.9734457253856),
 .UNSPECIFIED.);
#1331=B_SPLINE_CURVE_WITH_KNOTS('',3,(#11389,#11390,#11391,#11392,#11393,
#11394,#11395,#11396,#11397,#11398),.UNSPECIFIED.,.F.,.F.,(4,1,1,1,1,1,
1,4),(59.690260418206,60.2877689530072,61.2853695604035,62.2829701677998,
63.2805707751961,64.2781713825924,65.2757719899887,65.9734457253856),
 .UNSPECIFIED.);
#1332=B_SPLINE_CURVE_WITH_KNOTS('',3,(#11403,#11404,#11405,#11406,#11407,
#11408,#11409,#11410,#11411,#11412),.UNSPECIFIED.,.F.,.F.,(4,1,1,1,1,1,
1,4),(53.4070751110265,53.7608055149017,54.758406122298,55.7560067296943,
56.7536073370906,57.7512079444869,58.7488085518832,59.690260418206),
 .UNSPECIFIED.);
#1333=B_SPLINE_CURVE_WITH_KNOTS('',3,(#11413,#11414,#11415,#11416,#11417,
#11418,#11419,#11420,#11421,#11422),.UNSPECIFIED.,.F.,.F.,(4,1,1,1,1,1,
1,4),(53.4070751110265,54.3021653086293,55.2997659160256,56.2973665234219,
57.2949671308182,58.2925677382145,59.2901683456108,59.690260418206),
 .UNSPECIFIED.);
#1334=B_SPLINE_CURVE_WITH_KNOTS('',3,(#11427,#11428,#11429,#11430,#11431,
#11432,#11433,#11434,#11435,#11436),.UNSPECIFIED.,.F.,.F.,(4,1,1,1,1,1,
1,4),(47.1238898038469,47.7752018705238,48.7728024779201,49.7704030853164,
50.7680036927128,51.7656043001091,52.7632049075054,53.4070751110265),
 .UNSPECIFIED.);
#1335=B_SPLINE_CURVE_WITH_KNOTS('',3,(#11437,#11438,#11439,#11440,#11441,
#11442,#11443,#11444,#11445,#11446,#11447),.UNSPECIFIED.,.F.,.F.,(4,1,1,
1,1,1,1,1,4),(47.1238898038469,47.3189610568551,48.3165616642514,49.3141622716478,
50.3117628790441,51.3093634864404,52.3069640938367,53.304564701233,53.4070751110265),
 .UNSPECIFIED.);
#1336=B_SPLINE_CURVE_WITH_KNOTS('',3,(#11452,#11453,#11454,#11455,#11456,
#11457,#11458,#11459,#11460,#11461),.UNSPECIFIED.,.F.,.F.,(4,1,1,1,1,1,
1,4),(40.8407044966673,41.789598226146,42.7871988335423,43.7847994409386,
44.7824000483349,45.7800006557312,46.7776012631275,47.1238898038469),
 .UNSPECIFIED.);
#1337=B_SPLINE_CURVE_WITH_KNOTS('',3,(#11462,#11463,#11464,#11465,#11466,
#11467,#11468,#11469,#11470,#11471),.UNSPECIFIED.,.F.,.F.,(4,1,1,1,1,1,
1,4),(40.8407044966673,41.3333574124773,42.3309580198736,43.3285586272699,
44.3261592346662,45.3237598420625,46.3213604494588,47.1238898038469),
 .UNSPECIFIED.);
#1338=B_SPLINE_CURVE_WITH_KNOTS('',3,(#11476,#11477,#11478,#11479,#11480,
#11481,#11482,#11483,#11484,#11485,#11486),.UNSPECIFIED.,.F.,.F.,(4,1,1,
1,1,1,1,1,4),(34.5575191894877,34.8063939743718,35.8039945817681,36.8015951891644,
37.7991957965607,38.796796403957,39.7943970113533,40.7919976187497,40.8407044966673),
 .UNSPECIFIED.);
#1339=B_SPLINE_CURVE_WITH_KNOTS('',3,(#11487,#11488,#11489,#11490,#11491,
#11492,#11493,#11494,#11495,#11496),.UNSPECIFIED.,.F.,.F.,(4,1,1,1,1,1,
1,4),(34.5575191894877,35.3477537680994,36.3453543754957,37.342954982892,
38.3405555902884,39.3381561976847,40.335756805081,40.8407044966673),
 .UNSPECIFIED.);
#1340=B_SPLINE_CURVE_WITH_KNOTS('',3,(#11501,#11502,#11503,#11504,#11505,
#11506,#11507,#11508,#11509,#11510),.UNSPECIFIED.,.F.,.F.,(4,1,1,1,1,1,
1,4),(28.2743338823081,28.8207903299939,29.8183909373903,30.8159915447866,
31.8135921521829,32.8111927595792,33.8087933669755,34.5575191894877),
 .UNSPECIFIED.);
#1341=B_SPLINE_CURVE_WITH_KNOTS('',3,(#11511,#11512,#11513,#11514,#11515,
#11516,#11517,#11518,#11519,#11520,#11521),.UNSPECIFIED.,.F.,.F.,(4,1,1,
1,1,1,1,1,4),(28.2743338823081,28.3645495163253,29.3621501237216,30.3597507311179,
31.3573513385142,32.3549519459105,33.3525525533068,34.3501531607031,34.5575191894877),
 .UNSPECIFIED.);
#1342=B_SPLINE_CURVE_WITH_KNOTS('',3,(#11526,#11527,#11528,#11529,#11530,
#11531,#11532,#11533,#11534,#11535),.UNSPECIFIED.,.F.,.F.,(4,1,1,1,1,1,
1,4),(21.9911485751285,22.8351866856161,23.8327872930124,24.8303879004087,
25.827988507805,26.8255891152013,27.8231897225976,28.2743338823081),
 .UNSPECIFIED.);
#1343=B_SPLINE_CURVE_WITH_KNOTS('',3,(#11536,#11537,#11538,#11539,#11540,
#11541,#11542,#11543,#11544,#11545),.UNSPECIFIED.,.F.,.F.,(4,1,1,1,1,1,
1,4),(21.9911485751285,22.3789458719474,23.3765464793437,24.37414708674,
25.3717476941363,26.3693483015326,27.366948908929,28.2743338823081),
 .UNSPECIFIED.);
#1344=B_SPLINE_CURVE_WITH_KNOTS('',3,(#11551,#11552,#11553,#11554,#11555),
 .UNSPECIFIED.,.F.,.F.,(4,1,4),(14.3981410127769,15.3957416201732,15.7079632679489),
 .UNSPECIFIED.);
#1345=B_SPLINE_CURVE_WITH_KNOTS('',3,(#11558,#11559,#11560,#11561,#11562),
 .UNSPECIFIED.,.F.,.F.,(4,1,4),(13.8761928695311,14.8543818264456,15.7079632679489),
 .UNSPECIFIED.);
#1346=B_SPLINE_CURVE_WITH_KNOTS('',3,(#11639,#11640,#11641,#11642,#11643,
#11644,#11645,#11646,#11647,#11648),.UNSPECIFIED.,.F.,.F.,(4,2,2,2,4),(-0.768826429832705,
-0.767240199593363,-0.57329716583777,-0.461315679430967,-0.383620099794532),
 .UNSPECIFIED.);
#1347=B_SPLINE_CURVE_WITH_KNOTS('',3,(#11649,#11650,#11651,#11652,#11653,
#11654,#11655,#11656,#11657,#11658),.UNSPECIFIED.,.F.,.F.,(4,2,2,2,4),(-0.383620099794532,
-0.305924520158085,-0.193943033751236,0.,0.00158623023937601),
 .UNSPECIFIED.);
#1348=B_SPLINE_CURVE_WITH_KNOTS('',3,(#11669,#11670,#11671,#11672,#11673,
#11674,#11675,#11676,#11677,#11678,#11679,#11680,#11681,#11682,#11683,#11684,
#11685,#11686),.UNSPECIFIED.,.F.,.F.,(4,2,2,2,2,2,2,2,4),(-0.76882642980026,
-0.76724019956098,-0.573297165814677,-0.461315679413209,-0.383620099780493,
-0.305924520147777,-0.193943033746308,0.,0.00158623023927986),
 .UNSPECIFIED.);
#1349=B_SPLINE_CURVE_WITH_KNOTS('',3,(#11723,#11724,#11725,#11726,#11727,
#11728,#11729,#11730,#11731,#11732,#11733),.UNSPECIFIED.,.F.,.F.,(4,1,1,
1,1,1,1,1,4),(15.7079632679489,15.8519824338419,16.8495830412382,17.8471836486345,
18.8447842560309,19.8423848634272,20.8399854708235,21.8375860782198,21.9911485751285),
 .UNSPECIFIED.);
#1350=B_SPLINE_CURVE_WITH_KNOTS('',3,(#11734,#11735,#11736,#11737,#11738,
#11739,#11740,#11741,#11742,#11743),.UNSPECIFIED.,.F.,.F.,(4,1,1,1,1,1,
1,4),(15.7079632679489,16.3933422275696,17.3909428349659,18.3885434423622,
19.3861440497585,20.3837446571548,21.3813452645511,21.9911485751285),
 .UNSPECIFIED.);
#1351=B_SPLINE_CURVE_WITH_KNOTS('',3,(#12052,#12053,#12054,#12055,#12056,
#12057,#12058,#12059,#12060,#12061,#12062,#12063,#12064,#12065,#12066,#12067,
#12068,#12069,#12070,#12071,#12072,#12073,#12074,#12075,#12076,#12077,#12078,
#12079,#12080,#12081,#12082,#12083,#12084,#12085,#12086,#12087,#12088,#12089,
#12090,#12091,#12092,#12093,#12094,#12095,#12096,#12097,#12098,#12099,#12100,
#12101,#12102,#12103,#12104,#12105,#12106,#12107,#12108,#12109,#12110,#12111,
#12112,#12113,#12114,#12115,#12116,#12117,#12118,#12119,#12120,#12121,#12122,
#12123,#12124,#12125,#12126,#12127,#12128,#12129,#12130,#12131,#12132,#12133,
#12134,#12135,#12136),.UNSPECIFIED.,.F.,.F.,(4,3,3,3,3,3,3,3,3,3,3,3,3,
3,3,3,3,3,3,3,3,3,3,3,3,3,3,3,4),(0.,0.0219686281715528,0.0445463606193457,
0.0636242036118209,0.07209744784919,0.0767548581315063,0.0810487310113372,
0.102995303995266,0.124770867091271,0.14287042645824,0.150424219747402,
0.153922407205223,0.157567539717946,0.178337434372214,0.197169104559147,
0.219441601244649,0.224346217653563,0.229396798853662,0.250061927167916,
0.270722751313313,0.28567879435863,0.29689604993752,0.300623771856885,0.320395161135708,
0.334310894762281,0.33877647602486,0.357799721593331,0.375349078043162,
0.378621596831385),.UNSPECIFIED.);
#1352=B_SPLINE_CURVE_WITH_KNOTS('',3,(#12137,#12138,#12139,#12140,#12141,
#12142,#12143,#12144,#12145,#12146,#12147,#12148,#12149,#12150,#12151,#12152,
#12153,#12154,#12155,#12156,#12157,#12158,#12159,#12160,#12161,#12162,#12163,
#12164,#12165,#12166,#12167,#12168,#12169,#12170,#12171,#12172,#12173,#12174,
#12175,#12176,#12177,#12178,#12179,#12180,#12181,#12182,#12183,#12184,#12185,
#12186,#12187,#12188,#12189,#12190,#12191,#12192,#12193,#12194),
 .UNSPECIFIED.,.F.,.F.,(4,3,3,3,3,3,3,3,3,3,3,3,3,3,3,3,3,3,3,4),(-0.254990279232818,
-0.234477349668193,-0.22871674086773,-0.22506482824537,-0.203760387757535,
-0.200823997383662,-0.180338507409432,-0.158296763353209,-0.154234245100677,
-0.150791656345001,-0.129409593000311,-0.107575878454977,-0.0856092981050521,
-0.0801787505710101,-0.0759363781823176,-0.0533889982303693,-0.0308167874784648,
-0.00875888267892488,-0.00400455495965136,0.),.UNSPECIFIED.);
#1353=B_SPLINE_CURVE_WITH_KNOTS('',3,(#12195,#12196,#12197,#12198,#12199,
#12200,#12201,#12202,#12203,#12204,#12205,#12206,#12207,#12208,#12209,#12210,
#12211,#12212,#12213,#12214,#12215,#12216,#12217,#12218,#12219,#12220,#12221,
#12222),.UNSPECIFIED.,.F.,.F.,(4,3,3,3,3,3,3,3,3,4),(0.,0.0187208397268737,
0.0379355165382035,0.0581727843953796,0.0646638548438618,0.068387447778056,
0.0884839760262796,0.108890832871008,0.118884587966908,0.123178515106518),
 .UNSPECIFIED.);
#1354=B_SPLINE_CURVE_WITH_KNOTS('',3,(#12223,#12224,#12225,#12226,#12227,
#12228,#12229,#12230,#12231,#12232,#12233,#12234,#12235,#12236,#12237,#12238,
#12239,#12240,#12241,#12242,#12243,#12244,#12245,#12246,#12247),
 .UNSPECIFIED.,.F.,.F.,(4,3,3,3,3,3,3,3,4),(-10.1295685708718,-9.97600607396309,
-8.97840546656679,-7.98080485917047,-6.98320425177416,-5.98560364437785,
-4.98800303698155,-3.99040242958524,-3.84638326369224),.UNSPECIFIED.);
#1355=B_SPLINE_CURVE_WITH_KNOTS('',3,(#12556,#12557,#12558,#12559,#12560,
#12561,#12562,#12563,#12564,#12565,#12566,#12567,#12568,#12569,#12570,#12571,
#12572,#12573,#12574,#12575,#12576,#12577,#12578,#12579,#12580,#12581,#12582,
#12583,#12584,#12585,#12586,#12587,#12588,#12589,#12590,#12591,#12592,#12593,
#12594,#12595,#12596,#12597,#12598,#12599,#12600,#12601,#12602,#12603,#12604,
#12605,#12606,#12607,#12608,#12609,#12610,#12611,#12612,#12613,#12614,#12615,
#12616,#12617,#12618,#12619,#12620,#12621,#12622,#12623,#12624,#12625,#12626,
#12627,#12628,#12629,#12630,#12631,#12632,#12633,#12634,#12635,#12636,#12637),
 .UNSPECIFIED.,.F.,.F.,(4,3,3,3,3,3,3,3,3,3,3,3,3,3,3,3,3,3,3,3,3,3,3,3,
3,3,3,4),(0.,0.018600500233587,0.0384267791159037,0.0557747731379309,0.0644820401543133,
0.0684532947198101,0.0885096834401049,0.108920567554616,0.125993108488993,
0.133863030521655,0.137292306314217,0.158366893382889,0.177210731292121,
0.197737113300186,0.205654657471879,0.209128422925177,0.230132266768946,
0.251623567767457,0.26806575224317,0.278297158812869,0.284047681225798,
0.306316607432633,0.322975646846552,0.328163948660732,0.333182233583271,
0.355703596008113,0.372952765088309,0.376940817211645),.UNSPECIFIED.);
#1356=B_SPLINE_CURVE_WITH_KNOTS('',3,(#12638,#12639,#12640,#12641,#12642,
#12643,#12644,#12645,#12646,#12647,#12648,#12649,#12650,#12651,#12652,#12653,
#12654,#12655,#12656,#12657,#12658,#12659),.UNSPECIFIED.,.F.,.F.,(4,3,3,
3,3,3,3,4),(7.59300756235153,7.98080485917048,8.97840546656679,9.97600607396309,
10.9736066813594,11.9712072887557,12.968807896152,13.8761928695311),
 .UNSPECIFIED.);
#1357=B_SPLINE_CURVE_WITH_KNOTS('',3,(#12660,#12661,#12662,#12663,#12664,
#12665,#12666,#12667,#12668,#12669,#12670,#12671,#12672,#12673,#12674,#12675,
#12676,#12677,#12678,#12679,#12680,#12681,#12682,#12683,#12684,#12685,#12686,
#12687,#12688,#12689,#12690,#12691,#12692,#12693,#12694,#12695,#12696,#12697,
#12698,#12699,#12700,#12701,#12702,#12703,#12704,#12705,#12706,#12707,#12708,
#12709,#12710,#12711,#12712,#12713,#12714,#12715,#12716,#12717,#12718,#12719,
#12720,#12721,#12722,#12723,#12724,#12725,#12726,#12727,#12728,#12729,#12730,
#12731,#12732,#12733,#12734,#12735,#12736,#12737,#12738,#12739,#12740,#12741,
#12742,#12743,#12744),.UNSPECIFIED.,.F.,.F.,(4,3,3,3,3,3,3,3,3,3,3,3,3,
3,3,3,3,3,3,3,3,3,3,3,3,3,3,3,4),(-0.376940817211633,-0.354632454605328,
-0.332909565818261,-0.328060951840561,-0.305812359536112,-0.290191982632697,
-0.284249623441465,-0.278601398679216,-0.256918509535175,-0.235701747786141,
-0.214950060594018,-0.208208596987869,-0.204399741431515,-0.183824490029494,
-0.18084934430879,-0.159866544269734,-0.140290797877594,-0.135946608670285,
-0.132579097133426,-0.112119588209322,-0.0917553067258466,-0.0718282862666161,
-0.0676047210534115,-0.063655156602234,-0.0440979256320563,-0.0249133932463398,
-0.0063528163125237,-0.00326057313262047,0.),.UNSPECIFIED.);
#1358=B_SPLINE_CURVE_WITH_KNOTS('',3,(#12782,#12783,#12784,#12785,#12786,
#12787,#12788,#12789,#12790,#12791,#12792,#12793,#12794,#12795,#12796,#12797,
#12798,#12799,#12800,#12801,#12802,#12803,#12804,#12805,#12806,#12807,#12808,
#12809,#12810,#12811,#12812,#12813,#12814,#12815,#12816,#12817,#12818,#12819,
#12820,#12821,#12822,#12823,#12824,#12825,#12826,#12827,#12828,#12829,#12830,
#12831,#12832,#12833,#12834,#12835,#12836,#12837,#12838,#12839,#12840,#12841,
#12842,#12843,#12844,#12845,#12846,#12847,#12848,#12849,#12850,#12851,#12852,
#12853,#12854,#12855,#12856,#12857,#12858,#12859,#12860,#12861,#12862,#12863,
#12864,#12865,#12866),.UNSPECIFIED.,.F.,.F.,(4,3,3,3,3,3,3,3,3,3,3,3,3,
3,3,3,3,3,3,3,3,3,3,3,3,3,3,3,4),(0.,0.021968619134099,0.0445463508138711,
0.0636241950320315,0.0720974452774801,0.0767548527122233,0.0810487295372733,
0.102995302809976,0.124770868754624,0.142870427705757,0.150424219455889,
0.153922404976729,0.157567538938561,0.178337436410292,0.197169104559154,
0.219441601244656,0.22434621853845,0.229396798911011,0.250061926915346,
0.270722751583954,0.285678803759607,0.296896065746556,0.300623776312427,
0.320395169261119,0.334310908061463,0.33877648878019,0.357799740024219,
0.375349078043172,0.378621596831398),.UNSPECIFIED.);
#1359=B_SPLINE_CURVE_WITH_KNOTS('',3,(#12867,#12868,#12869,#12870,#12871,
#12872,#12873,#12874,#12875,#12876,#12877,#12878,#12879,#12880,#12881,#12882,
#12883,#12884,#12885,#12886,#12887,#12888,#12889,#12890,#12891,#12892,#12893,
#12894,#12895,#12896,#12897,#12898,#12899,#12900,#12901,#12902,#12903,#12904,
#12905,#12906,#12907,#12908,#12909,#12910,#12911,#12912,#12913,#12914,#12915,
#12916,#12917,#12918,#12919,#12920,#12921,#12922,#12923,#12924,#12925,#12926,
#12927,#12928,#12929,#12930,#12931,#12932,#12933,#12934,#12935,#12936,#12937,
#12938,#12939,#12940,#12941,#12942,#12943,#12944,#12945,#12946,#12947,#12948),
 .UNSPECIFIED.,.F.,.F.,(4,3,3,3,3,3,3,3,3,3,3,3,3,3,3,3,3,3,3,3,3,3,3,3,
3,3,3,4),(0.,0.0186005373117356,0.038426811559284,0.0557748015258888,0.0644820892685102,
0.0684533078055671,0.0885097227040427,0.108920617705581,0.125993146102217,
0.133863089681963,0.137292338809663,0.158366921726846,0.177210731292123,
0.197737094100997,0.205654646587328,0.20912841497494,0.23013223615724,0.251623525403939,
0.268065761427934,0.278297179882888,0.284047675336949,0.306316600241872,
0.32297564145348,0.328163936759366,0.333182227701541,0.355703590029263,
0.372952765088304,0.37694081721164),.UNSPECIFIED.);
#1360=B_SPLINE_CURVE_WITH_KNOTS('',3,(#12949,#12950,#12951,#12952,#12953,
#12954,#12955,#12956,#12957,#12958,#12959,#12960,#12961,#12962,#12963,#12964,
#12965,#12966,#12967,#12968,#12969,#12970,#12971,#12972,#12973,#12974,#12975,
#12976,#12977,#12978,#12979,#12980,#12981,#12982,#12983,#12984,#12985,#12986,
#12987,#12988,#12989,#12990,#12991,#12992,#12993,#12994,#12995,#12996,#12997,
#12998,#12999,#13000,#13001,#13002,#13003,#13004,#13005,#13006,#13007,#13008,
#13009,#13010,#13011,#13012,#13013,#13014,#13015,#13016,#13017,#13018,#13019,
#13020,#13021,#13022,#13023,#13024,#13025,#13026,#13027,#13028,#13029,#13030,
#13031,#13032,#13033),.UNSPECIFIED.,.F.,.F.,(4,3,3,3,3,3,3,3,3,3,3,3,3,
3,3,3,3,3,3,3,3,3,3,3,3,3,3,3,4),(0.,0.0219686380514027,0.0445463713382339,
0.0636242129908502,0.0720974506611356,0.0767548640568597,0.0810487326131753,
0.102995305281134,0.124770865263899,0.142870425087715,0.150424220061154,
0.153922409603196,0.157567540562184,0.178337432135944,0.197169104559165,
0.219441601244671,0.224346216685054,0.229396798808629,0.250061927461599,
0.270722751034184,0.285678784130498,0.296896032726582,0.300623767000752,
0.320395152261939,0.334310880229888,0.338776462161233,0.357799701520601,
0.375349078043213,0.378621596831437),.UNSPECIFIED.);
#1361=B_SPLINE_CURVE_WITH_KNOTS('',3,(#13034,#13035,#13036,#13037,#13038,
#13039,#13040,#13041,#13042,#13043,#13044,#13045,#13046,#13047,#13048,#13049,
#13050,#13051,#13052,#13053,#13054,#13055,#13056,#13057,#13058,#13059,#13060,
#13061,#13062,#13063,#13064,#13065,#13066,#13067,#13068,#13069,#13070,#13071,
#13072,#13073,#13074,#13075,#13076,#13077,#13078,#13079,#13080,#13081,#13082,
#13083,#13084,#13085,#13086,#13087,#13088,#13089,#13090,#13091,#13092,#13093,
#13094,#13095,#13096,#13097,#13098,#13099,#13100,#13101,#13102,#13103,#13104,
#13105,#13106,#13107,#13108,#13109,#13110,#13111,#13112,#13113,#13114,#13115),
 .UNSPECIFIED.,.F.,.F.,(4,3,3,3,3,3,3,3,3,3,3,3,3,3,3,3,3,3,3,3,3,3,3,3,
3,3,3,4),(0.,0.0186005115768008,0.038426789041218,0.055774781822583,0.06448205517952,
0.0684532987383391,0.088509695468686,0.108920582912668,0.125993120007535,
0.133863048637895,0.137292316222759,0.158366902021944,0.177210731292138,
0.197737107427825,0.205654654143849,0.209128420488014,0.230132257400709,
0.251623554805102,0.268065755057508,0.278297165271629,0.284047679418564,
0.306316605227149,0.322975645192443,0.328163945080186,0.333182231795999,
0.355703594193589,0.372952765088323,0.376940817211659),.UNSPECIFIED.);
#1362=B_SPLINE_CURVE_WITH_KNOTS('',3,(#13116,#13117,#13118,#13119,#13120,
#13121,#13122,#13123,#13124,#13125,#13126,#13127,#13128,#13129,#13130,#13131,
#13132,#13133,#13134,#13135,#13136,#13137,#13138,#13139,#13140,#13141,#13142,
#13143,#13144,#13145,#13146,#13147,#13148,#13149,#13150,#13151,#13152,#13153,
#13154,#13155,#13156,#13157,#13158,#13159,#13160,#13161,#13162,#13163,#13164,
#13165,#13166,#13167,#13168,#13169,#13170,#13171,#13172,#13173,#13174,#13175,
#13176,#13177,#13178,#13179,#13180,#13181,#13182,#13183,#13184,#13185,#13186,
#13187,#13188,#13189,#13190,#13191,#13192,#13193,#13194,#13195,#13196,#13197,
#13198,#13199,#13200),.UNSPECIFIED.,.F.,.F.,(4,3,3,3,3,3,3,3,3,3,3,3,3,
3,3,3,3,3,3,3,3,3,3,3,3,3,3,3,4),(0.,0.0219686109476892,0.0445463419311616,
0.0636241872596606,0.072097442945625,0.0767548477970364,0.0810487282633608,
0.102995301796811,0.124770870320527,0.142870428880184,0.150424219224462,
0.15392240302136,0.157567538243027,0.178337438267784,0.197169104559153,
0.219441601244657,0.224346219340572,0.229396798953165,0.250061926675953,
0.270722751817935,0.285678812243067,0.296896080015907,0.300623780338084,
0.320395176613474,0.334310920099279,0.338776500225901,0.357799756613675,
0.375349078043179,0.378621596831404),.UNSPECIFIED.);
#1363=B_SPLINE_CURVE_WITH_KNOTS('',3,(#13201,#13202,#13203,#13204,#13205,
#13206,#13207,#13208,#13209,#13210,#13211,#13212,#13213,#13214,#13215,#13216,
#13217,#13218,#13219,#13220,#13221,#13222,#13223,#13224,#13225,#13226,#13227,
#13228,#13229,#13230,#13231,#13232,#13233,#13234,#13235,#13236,#13237,#13238,
#13239,#13240,#13241,#13242,#13243,#13244,#13245,#13246,#13247,#13248,#13249,
#13250,#13251,#13252,#13253,#13254,#13255,#13256,#13257,#13258,#13259,#13260,
#13261,#13262,#13263,#13264,#13265,#13266,#13267,#13268,#13269,#13270,#13271,
#13272,#13273,#13274,#13275,#13276,#13277,#13278,#13279,#13280,#13281,#13282),
 .UNSPECIFIED.,.F.,.F.,(4,3,3,3,3,3,3,3,3,3,3,3,3,3,3,3,3,3,3,3,3,3,3,3,
3,3,3,4),(0.,0.0186005239390001,0.0384267998581411,0.0557747912873894,0.0644820715548053,
0.0684533030913493,0.0885097085463574,0.108920599618628,0.125993132537003,
0.133863068345662,0.137292327044492,0.158366911460439,0.177210731292128,
0.197737101028813,0.205654650516969,0.209128417840175,0.230132247197424,
0.251623540683617,0.268065758119471,0.278297172296056,0.284047677474677,
0.306316602850204,0.322975643409731,0.328163941106245,0.333182229833608,
0.355703592197711,0.372952765088311,0.376940817211644),.UNSPECIFIED.);
#1364=B_SPLINE_CURVE_WITH_KNOTS('',3,(#13284,#13285,#13286,#13287,#13288,
#13289,#13290,#13291,#13292,#13293,#13294),.UNSPECIFIED.,.F.,.F.,(4,1,1,
1,1,1,1,1,4),(15.7079632679489,15.8519824338419,16.8495830412382,17.8471836486345,
18.8447842560308,19.8423848634271,20.8399854708235,21.8375860782198,21.9911485751285),
 .UNSPECIFIED.);
#1365=B_SPLINE_CURVE_WITH_KNOTS('',3,(#13295,#13296,#13297,#13298,#13299,
#13300,#13301,#13302,#13303,#13304),.UNSPECIFIED.,.F.,.F.,(4,1,1,1,1,1,
1,4),(15.7079632679489,16.3933422275695,17.3909428349659,18.3885434423622,
19.3861440497585,20.3837446571548,21.3813452645511,21.9911485751285),
 .UNSPECIFIED.);
#1366=B_SPLINE_CURVE_WITH_KNOTS('',3,(#13613,#13614,#13615,#13616,#13617,
#13618,#13619,#13620,#13621,#13622,#13623,#13624,#13625,#13626,#13627,#13628,
#13629,#13630,#13631,#13632,#13633,#13634,#13635,#13636,#13637,#13638,#13639,
#13640,#13641,#13642,#13643,#13644,#13645,#13646,#13647,#13648,#13649,#13650,
#13651,#13652,#13653,#13654,#13655,#13656,#13657,#13658,#13659,#13660,#13661,
#13662,#13663,#13664,#13665,#13666,#13667,#13668,#13669,#13670,#13671,#13672,
#13673,#13674,#13675,#13676,#13677,#13678,#13679,#13680,#13681,#13682,#13683,
#13684,#13685,#13686,#13687,#13688,#13689,#13690,#13691,#13692,#13693,#13694,
#13695,#13696,#13697,#13698,#13699,#13700),.UNSPECIFIED.,.F.,.F.,(4,3,3,
3,3,3,3,3,3,3,3,3,3,3,3,3,3,3,3,3,3,3,3,3,3,3,3,3,3,4),(-0.378621596831427,
-0.359794625220292,-0.347847845255257,-0.339608528850609,-0.335317716276224,
-0.315442613111551,-0.301115286145566,-0.297116173616389,-0.293205026311676,
-0.272800449719613,-0.252103127039742,-0.239283344625725,-0.22876814535061,
-0.224492807264877,-0.203188357883528,-0.200823997383671,-0.180338493313755,
-0.158296751019492,-0.154234157832905,-0.15079163756267,-0.12940956273182,
-0.107575843179879,-0.0856092627735954,-0.0801786890662741,-0.0759363558949484,
-0.0533889736446962,-0.0308167632838699,-0.00875885575216316,-0.00400455495965028,
0.),.UNSPECIFIED.);
#1367=B_SPLINE_CURVE_WITH_KNOTS('',3,(#13701,#13702,#13703,#13704,#13705,
#13706,#13707,#13708,#13709,#13710,#13711,#13712,#13713,#13714,#13715,#13716,
#13717,#13718,#13719,#13720,#13721,#13722,#13723,#13724,#13725),
 .UNSPECIFIED.,.F.,.F.,(4,3,3,3,3,3,3,3,4),(-10.1295685708718,-9.97600607396309,
-8.97840546656678,-7.98080485917047,-6.98320425177416,-5.98560364437785,
-4.98800303698155,-3.99040242958523,-3.84638326369224),.UNSPECIFIED.);
#1368=B_SPLINE_CURVE_WITH_KNOTS('',3,(#14034,#14035,#14036,#14037,#14038,
#14039,#14040,#14041,#14042,#14043,#14044,#14045,#14046,#14047,#14048,#14049,
#14050,#14051,#14052,#14053,#14054,#14055),.UNSPECIFIED.,.F.,.F.,(4,3,3,
3,3,3,3,4),(7.59300756235153,7.98080485917047,8.97840546656678,9.9760060739631,
10.9736066813594,11.9712072887557,12.968807896152,13.8761928695311),
 .UNSPECIFIED.);
#1369=B_SPLINE_CURVE_WITH_KNOTS('',3,(#14056,#14057,#14058,#14059,#14060,
#14061,#14062,#14063,#14064,#14065,#14066,#14067,#14068,#14069,#14070,#14071,
#14072,#14073,#14074,#14075,#14076,#14077,#14078,#14079,#14080,#14081,#14082,
#14083,#14084,#14085,#14086,#14087,#14088,#14089,#14090,#14091,#14092,#14093,
#14094,#14095,#14096,#14097,#14098,#14099,#14100,#14101,#14102,#14103,#14104,
#14105,#14106,#14107,#14108,#14109,#14110,#14111,#14112,#14113,#14114,#14115,
#14116,#14117,#14118,#14119,#14120,#14121,#14122,#14123,#14124,#14125,#14126,
#14127,#14128,#14129,#14130,#14131,#14132,#14133,#14134,#14135,#14136,#14137,
#14138,#14139,#14140),.UNSPECIFIED.,.F.,.F.,(4,3,3,3,3,3,3,3,3,3,3,3,3,
3,3,3,3,3,3,3,3,3,3,3,3,3,3,3,4),(-0.376940817211658,-0.354632440305215,
-0.332909553305663,-0.328060937224979,-0.305812345362663,-0.29019197023093,
-0.284249595905682,-0.278601400527098,-0.25691851401837,-0.23570175863681,
-0.214950075630617,-0.208208587756039,-0.204399742947041,-0.183824497720044,
-0.180849344308799,-0.159866544391984,-0.140290797984564,-0.135946620453725,
-0.132579106908657,-0.11211959722078,-0.0917553180086424,-0.0718283063725309,
-0.0676047765030496,-0.0636551755593219,-0.0440979496009447,-0.0249134276262131,
-0.00635286745037528,-0.00326057313262046,0.),.UNSPECIFIED.);
#1370=B_SPLINE_CURVE_WITH_KNOTS('',3,(#14142,#14143,#14144,#14145,#14146,
#14147,#14148,#14149,#14150,#14151,#14152),.UNSPECIFIED.,.F.,.F.,(4,1,1,
1,1,1,1,1,4),(15.7079632679489,15.8519824338419,16.8495830412382,17.8471836486345,
18.8447842560308,19.8423848634271,20.8399854708235,21.8375860782198,21.9911485751285),
 .UNSPECIFIED.);
#1371=B_SPLINE_CURVE_WITH_KNOTS('',3,(#14153,#14154,#14155,#14156,#14157,
#14158,#14159,#14160,#14161,#14162),.UNSPECIFIED.,.F.,.F.,(4,1,1,1,1,1,
1,4),(15.7079632679489,16.3933422275695,17.3909428349659,18.3885434423622,
19.3861440497585,20.3837446571548,21.3813452645511,21.9911485751285),
 .UNSPECIFIED.);
#1372=B_SPLINE_CURVE_WITH_KNOTS('',3,(#14471,#14472,#14473,#14474,#14475,
#14476,#14477,#14478,#14479,#14480,#14481,#14482,#14483,#14484,#14485,#14486,
#14487,#14488,#14489,#14490,#14491,#14492,#14493,#14494,#14495,#14496,#14497,
#14498,#14499,#14500,#14501,#14502,#14503,#14504,#14505,#14506,#14507,#14508,
#14509,#14510,#14511,#14512,#14513,#14514,#14515,#14516,#14517,#14518,#14519,
#14520,#14521,#14522,#14523,#14524,#14525,#14526,#14527,#14528,#14529,#14530,
#14531,#14532,#14533,#14534,#14535,#14536,#14537,#14538,#14539,#14540,#14541,
#14542,#14543,#14544,#14545,#14546,#14547,#14548,#14549,#14550,#14551,#14552,
#14553,#14554,#14555,#14556,#14557,#14558),.UNSPECIFIED.,.F.,.F.,(4,3,3,
3,3,3,3,3,3,3,3,3,3,3,3,3,3,3,3,3,3,3,3,3,3,3,3,3,3,4),(-0.378621596831439,
-0.35979459391274,-0.347847765628199,-0.339607786177388,-0.335317210572095,
-0.315442075259891,-0.301114815525364,-0.297115056007226,-0.293204827194635,
-0.272800226631742,-0.25210290804161,-0.239283180377127,-0.228767902917728,
-0.22449272396701,-0.203188276512031,-0.200823997383678,-0.180338515496785,
-0.158296770429644,-0.154234295176689,-0.150791667121598,-0.129409610366437,
-0.107575898692758,-0.0856093183754116,-0.0801787858574953,-0.0759363909673205,
-0.0533890123327845,-0.0308168013567995,-0.00875889812582652,-0.00400455495965099,
0.),.UNSPECIFIED.);
#1373=B_SPLINE_CURVE_WITH_KNOTS('',3,(#14559,#14560,#14561,#14562,#14563,
#14564,#14565,#14566,#14567,#14568,#14569,#14570,#14571,#14572,#14573,#14574,
#14575,#14576,#14577,#14578,#14579,#14580,#14581,#14582,#14583),
 .UNSPECIFIED.,.F.,.F.,(4,3,3,3,3,3,3,3,4),(-10.1295685708718,-9.97600607396309,
-8.97840546656678,-7.98080485917047,-6.98320425177416,-5.98560364437785,
-4.98800303698155,-3.99040242958524,-3.84638326369225),.UNSPECIFIED.);
#1374=B_SPLINE_CURVE_WITH_KNOTS('',3,(#14892,#14893,#14894,#14895,#14896,
#14897,#14898,#14899,#14900,#14901,#14902,#14903,#14904,#14905,#14906,#14907,
#14908,#14909,#14910,#14911,#14912,#14913),.UNSPECIFIED.,.F.,.F.,(4,3,3,
3,3,3,3,4),(7.59300756235153,7.98080485917047,8.97840546656678,9.9760060739631,
10.9736066813594,11.9712072887557,12.968807896152,13.8761928695311),
 .UNSPECIFIED.);
#1375=B_SPLINE_CURVE_WITH_KNOTS('',3,(#14914,#14915,#14916,#14917,#14918,
#14919,#14920,#14921,#14922,#14923,#14924,#14925,#14926,#14927,#14928,#14929,
#14930,#14931,#14932,#14933,#14934,#14935,#14936,#14937,#14938,#14939,#14940,
#14941,#14942,#14943,#14944,#14945,#14946,#14947,#14948,#14949,#14950,#14951,
#14952,#14953,#14954,#14955,#14956,#14957,#14958,#14959,#14960,#14961,#14962,
#14963,#14964,#14965,#14966,#14967,#14968,#14969,#14970,#14971,#14972,#14973,
#14974,#14975,#14976,#14977,#14978,#14979,#14980,#14981,#14982,#14983,#14984,
#14985,#14986,#14987,#14988,#14989,#14990,#14991,#14992,#14993,#14994,#14995,
#14996,#14997,#14998),.UNSPECIFIED.,.F.,.F.,(4,3,3,3,3,3,3,3,3,3,3,3,3,
3,3,3,3,3,3,3,3,3,3,3,3,3,3,3,4),(-0.376940817211635,-0.354632447762244,
-0.332909559830562,-0.32806094484179,-0.305812352748728,-0.290191976693736,
-0.284249610255867,-0.278601399566055,-0.256918511682903,-0.235701752980436,
-0.214950067791438,-0.208208592568691,-0.204399742168023,-0.183824493720622,
-0.180849344308789,-0.159866544328361,-0.140290797928894,-0.135946614308445,
-0.132579101815663,-0.112119592526046,-0.0917553121288918,-0.0718282958900664,
-0.0676047475926938,-0.0636551656772768,-0.0440979371043374,-0.0249134096995733,
-0.00635284078267037,-0.00326057313262106,0.),.UNSPECIFIED.);
#1376=B_SPLINE_CURVE_WITH_KNOTS('',3,(#15000,#15001,#15002,#15003,#15004,
#15005,#15006,#15007,#15008,#15009,#15010),.UNSPECIFIED.,.F.,.F.,(4,1,1,
1,1,1,1,1,4),(15.7079632679489,15.8519824338419,16.8495830412382,17.8471836486345,
18.8447842560309,19.8423848634272,20.8399854708235,21.8375860782198,21.9911485751285),
 .UNSPECIFIED.);
#1377=B_SPLINE_CURVE_WITH_KNOTS('',3,(#15011,#15012,#15013,#15014,#15015,
#15016,#15017,#15018,#15019,#15020),.UNSPECIFIED.,.F.,.F.,(4,1,1,1,1,1,
1,4),(15.7079632679489,16.3933422275696,17.3909428349659,18.3885434423622,
19.3861440497585,20.3837446571548,21.3813452645511,21.9911485751285),
 .UNSPECIFIED.);
#1378=B_SPLINE_CURVE_WITH_KNOTS('',3,(#15329,#15330,#15331,#15332,#15333,
#15334,#15335,#15336,#15337,#15338,#15339,#15340,#15341,#15342,#15343,#15344,
#15345,#15346,#15347,#15348,#15349,#15350,#15351,#15352,#15353,#15354,#15355,
#15356,#15357,#15358,#15359,#15360,#15361,#15362,#15363,#15364,#15365,#15366,
#15367,#15368,#15369,#15370,#15371,#15372,#15373,#15374,#15375,#15376,#15377,
#15378,#15379,#15380,#15381,#15382,#15383,#15384,#15385,#15386,#15387,#15388,
#15389,#15390,#15391,#15392,#15393,#15394,#15395,#15396,#15397,#15398,#15399,
#15400,#15401,#15402,#15403,#15404,#15405,#15406,#15407,#15408,#15409,#15410,
#15411,#15412,#15413,#15414,#15415,#15416),.UNSPECIFIED.,.F.,.F.,(4,3,3,
3,3,3,3,3,3,3,3,3,3,3,3,3,3,3,3,3,3,3,3,3,3,3,3,3,3,4),(-0.378621596831402,
-0.359794615761403,-0.347847821197377,-0.339608304483908,-0.335317563605001,
-0.315442450729176,-0.301115144060986,-0.297115836250077,-0.293204966248274,
-0.272800382415427,-0.252103060970179,-0.23928329507355,-0.228768072211328,
-0.224492782138973,-0.203188333339894,-0.200823997383662,-0.180338500015385,
-0.158296756883418,-0.154234199332552,-0.150791646494627,-0.129409577124881,
-0.107575859953488,-0.0856092795738859,-0.0801787183117794,-0.0759363664912861,
-0.0533889853334927,-0.0308167747861896,-0.00875886855324413,-0.00400455495965136,
0.),.UNSPECIFIED.);
#1379=B_SPLINE_CURVE_WITH_KNOTS('',3,(#15417,#15418,#15419,#15420,#15421,
#15422,#15423,#15424,#15425,#15426,#15427,#15428,#15429,#15430,#15431,#15432,
#15433,#15434,#15435,#15436,#15437,#15438,#15439,#15440,#15441),
 .UNSPECIFIED.,.F.,.F.,(4,3,3,3,3,3,3,3,4),(-10.1295685708718,-9.97600607396309,
-8.97840546656678,-7.98080485917047,-6.98320425177416,-5.98560364437786,
-4.98800303698154,-3.99040242958524,-3.84638326369224),.UNSPECIFIED.);
#1380=B_SPLINE_CURVE_WITH_KNOTS('',3,(#15750,#15751,#15752,#15753,#15754,
#15755,#15756,#15757,#15758,#15759,#15760,#15761,#15762,#15763,#15764,#15765,
#15766,#15767,#15768,#15769,#15770,#15771),.UNSPECIFIED.,.F.,.F.,(4,3,3,
3,3,3,3,4),(7.59300756235153,7.98080485917048,8.97840546656678,9.9760060739631,
10.9736066813594,11.9712072887557,12.968807896152,13.8761928695311),
 .UNSPECIFIED.);
#1381=B_SPLINE_CURVE_WITH_KNOTS('',3,(#15772,#15773,#15774,#15775,#15776,
#15777,#15778,#15779,#15780,#15781,#15782,#15783,#15784,#15785,#15786,#15787,
#15788,#15789,#15790,#15791,#15792,#15793,#15794,#15795,#15796,#15797,#15798,
#15799,#15800,#15801,#15802),.UNSPECIFIED.,.F.,.F.,(4,3,3,3,3,3,3,3,3,3,
4),(0.050378130562488,0.0706766774202748,0.0909513952302104,0.110830379637232,
0.119055313841064,0.122780653122509,0.126719562075065,0.146060569004475,
0.164791269949457,0.170467332858295,0.173733289126884),.UNSPECIFIED.);
#1382=B_SPLINE_CURVE_WITH_KNOTS('',3,(#15803,#15804,#15805,#15806,#15807,
#15808,#15809,#15810,#15811,#15812,#15813,#15814,#15815,#15816,#15817,#15818,
#15819,#15820,#15821,#15822,#15823,#15824,#15825,#15826,#15827,#15828,#15829,
#15830,#15831,#15832,#15833,#15834,#15835,#15836,#15837,#15838,#15839,#15840,
#15841,#15842,#15843,#15844,#15845,#15846,#15847,#15848,#15849,#15850,#15851,
#15852,#15853,#15854,#15855,#15856,#15857,#15858,#15859,#15860),
 .UNSPECIFIED.,.F.,.F.,(4,3,3,3,3,3,3,3,3,3,3,3,3,3,3,3,3,3,3,4),(-0.376940817211632,
-0.354632432238001,-0.332909546246849,-0.328060928965978,-0.305812337354451,
-0.290191963223743,-0.284249580349225,-0.278601401578559,-0.256918516557476,
-0.235701764768698,-0.214950084124798,-0.20820858254272,-0.204399743801857,
-0.183824502058691,-0.18084934430879,-0.159816080827987,-0.141544175656564,
-0.136361698528752,-0.132490636717292,-0.123272270485141),.UNSPECIFIED.);
#1383=B_SPLINE_CURVE_WITH_KNOTS('',3,(#16353,#16354,#16355,#16356,#16357,
#16358,#16359,#16360,#16361,#16362),.UNSPECIFIED.,.F.,.F.,(4,3,3,4),(-4.09254174883832,
-3.98935377563313,-2.99201533172485,-2.06514013327812),.UNSPECIFIED.);
#1384=B_SPLINE_CURVE_WITH_KNOTS('',3,(#16365,#16366,#16367,#16368,#16369,
#16370,#16371),.UNSPECIFIED.,.F.,.F.,(4,3,4),(0.,0.998359650364244,1.11419103802955),
 .UNSPECIFIED.);
#1385=B_SPLINE_CURVE_WITH_KNOTS('',3,(#16376,#16377,#16378,#16379,#16380,
#16381,#16382,#16383,#16384,#16385,#16386,#16387,#16388,#16389,#16390,#16391,
#16392,#16393,#16394,#16395,#16396,#16397),.UNSPECIFIED.,.F.,.F.,(4,3,3,
3,3,3,3,4),(-10.3757270560179,-9.97338443908282,-8.97604599517454,-7.97870755126626,
-6.98136910735798,-5.98403066344969,-4.98669221954141,-4.09254174883832),
 .UNSPECIFIED.);
#1386=B_SPLINE_CURVE_WITH_KNOTS('',3,(#16398,#16399,#16400,#16401,#16402,
#16403,#16404,#16405,#16406,#16407,#16408,#16409,#16410,#16411,#16412,#16413,
#16414,#16415,#16416,#16417,#16418,#16419),.UNSPECIFIED.,.F.,.F.,(4,3,3,
3,3,3,3,4),(1.11419103802955,1.99671930072849,2.99507895109274,3.99343860145699,
4.99179825182123,5.99015790218548,6.98851755254973,7.39737634520914),
 .UNSPECIFIED.);
#1387=B_SPLINE_CURVE_WITH_KNOTS('',3,(#16424,#16425,#16426,#16427,#16428,
#16429,#16430,#16431,#16432,#16433,#16434,#16435,#16436,#16437,#16438,#16439,
#16440,#16441,#16442,#16443,#16444,#16445),.UNSPECIFIED.,.F.,.F.,(4,3,3,
3,3,3,3,4),(-16.6589123631975,-15.9574151025325,-14.9600766586242,-13.962738214716,
-12.9653997708077,-11.9680613268994,-10.9707228829911,-10.3757270560179),
 .UNSPECIFIED.);
#1388=B_SPLINE_CURVE_WITH_KNOTS('',3,(#16446,#16447,#16448,#16449,#16450,
#16451,#16452,#16453,#16454,#16455,#16456,#16457,#16458,#16459,#16460,#16461,
#16462,#16463,#16464,#16465,#16466,#16467),.UNSPECIFIED.,.F.,.F.,(4,3,3,
3,3,3,3,4),(7.39737634520914,7.98687720291397,8.98523685327822,9.98359650364247,
10.9819561540067,11.980315804371,12.9786754547352,13.6805616523887),
 .UNSPECIFIED.);
#1389=B_SPLINE_CURVE_WITH_KNOTS('',3,(#16472,#16473,#16474,#16475,#16476,
#16477,#16478,#16479,#16480,#16481,#16482,#16483,#16484,#16485,#16486,#16487,
#16488,#16489,#16490,#16491,#16492,#16493,#16494,#16495,#16496),
 .UNSPECIFIED.,.F.,.F.,(4,3,3,3,3,3,3,3,4),(-22.9420976703771,-22.9387842098905,
-21.9414457659822,-20.9441073220739,-19.9467688781656,-18.9494304342574,
-17.9520919903491,-16.9547535464408,-16.6589123631975),.UNSPECIFIED.);
#1390=B_SPLINE_CURVE_WITH_KNOTS('',3,(#16497,#16498,#16499,#16500,#16501,
#16502,#16503,#16504,#16505,#16506,#16507,#16508,#16509,#16510,#16511,#16512,
#16513,#16514,#16515,#16516,#16517,#16518),.UNSPECIFIED.,.F.,.F.,(4,3,3,
3,3,3,3,4),(13.6805616523887,13.9770351050995,14.9753947554637,15.973754405828,
16.9721140561922,17.9704737065565,18.9688333569207,19.9637469595683),
 .UNSPECIFIED.);
#1391=B_SPLINE_CURVE_WITH_KNOTS('',3,(#16523,#16524,#16525,#16526,#16527,
#16528,#16529,#16530,#16531,#16532,#16533,#16534,#16535,#16536,#16537,#16538,
#16539,#16540,#16541,#16542,#16543,#16544),.UNSPECIFIED.,.F.,.F.,(4,3,3,
3,3,3,3,4),(-29.2252829775567,-28.9228148733402,-27.9254764294319,-26.9281379855236,
-25.9307995416153,-24.9334610977071,-23.9361226537988,-22.9420976703771),
 .UNSPECIFIED.);
#1392=B_SPLINE_CURVE_WITH_KNOTS('',3,(#16545,#16546,#16547,#16548,#16549,
#16550,#16551,#16552,#16553,#16554,#16555,#16556,#16557,#16558,#16559,#16560,
#16561,#16562,#16563,#16564,#16565,#16566,#16567,#16568,#16569),
 .UNSPECIFIED.,.F.,.F.,(4,3,3,3,3,3,3,3,4),(19.9637469595683,19.967193007285,
20.9655526576492,21.9639123080134,22.9622719583777,23.9606316087419,24.9589912591062,
25.9573509094704,26.2469322667479),.UNSPECIFIED.);
#1393=B_SPLINE_CURVE_WITH_KNOTS('',3,(#16574,#16575,#16576,#16577,#16578,
#16579,#16580,#16581,#16582,#16583,#16584,#16585,#16586,#16587,#16588,#16589,
#16590,#16591,#16592,#16593,#16594,#16595),.UNSPECIFIED.,.F.,.F.,(4,3,3,
3,3,3,3,4),(-35.5084682847363,-34.9068455367899,-33.9095070928816,-32.9121686489733,
-31.914830205065,-30.9174917611567,-29.9201533172485,-29.2252829775567),
 .UNSPECIFIED.);
#1394=B_SPLINE_CURVE_WITH_KNOTS('',3,(#16596,#16597,#16598,#16599,#16600,
#16601,#16602,#16603,#16604,#16605,#16606,#16607,#16608,#16609,#16610,#16611,
#16612,#16613,#16614,#16615,#16616,#16617),.UNSPECIFIED.,.F.,.F.,(4,3,3,
3,3,3,3,4),(26.2469322667479,26.9557105598347,27.9540702101989,28.9524298605632,
29.9507895109274,30.9491491612917,31.9475088116559,32.5301175739275),
 .UNSPECIFIED.);
#1395=B_SPLINE_CURVE_WITH_KNOTS('',3,(#16622,#16623,#16624,#16625,#16626,
#16627,#16628,#16629,#16630,#16631,#16632,#16633,#16634,#16635,#16636,#16637,
#16638,#16639,#16640,#16641,#16642,#16643),.UNSPECIFIED.,.F.,.F.,(4,3,3,
3,3,3,3,4),(-41.7916535919158,-40.8908762002396,-39.8935377563313,-38.896199312423,
-37.8988608685147,-36.9015224246064,-35.9041839806982,-35.5084682847363),
 .UNSPECIFIED.);
#1396=B_SPLINE_CURVE_WITH_KNOTS('',3,(#16644,#16645,#16646,#16647,#16648,
#16649,#16650,#16651,#16652,#16653,#16654,#16655,#16656,#16657,#16658,#16659,
#16660,#16661,#16662,#16663,#16664,#16665),.UNSPECIFIED.,.F.,.F.,(4,3,3,
3,3,3,3,4),(32.5301175739275,32.9458684620202,33.9442281123844,34.9425877627486,
35.9409474131129,36.9393070634771,37.9376667138414,38.8133028811071),
 .UNSPECIFIED.);
#1397=B_SPLINE_CURVE_WITH_KNOTS('',3,(#16670,#16671,#16672,#16673,#16674,
#16675,#16676,#16677,#16678,#16679,#16680,#16681,#16682,#16683,#16684,#16685,
#16686,#16687,#16688,#16689,#16690,#16691,#16692,#16693,#16694),
 .UNSPECIFIED.,.F.,.F.,(4,3,3,3,3,3,3,3,4),(-48.0748388990954,-47.8722453075976,
-46.8749068636893,-45.877568419781,-44.8802299758727,-43.8828915319644,
-42.8855530880561,-41.8882146441479,-41.7916535919158),.UNSPECIFIED.);
#1398=B_SPLINE_CURVE_WITH_KNOTS('',3,(#16695,#16696,#16697,#16698,#16699,
#16700,#16701,#16702,#16703,#16704,#16705,#16706,#16707,#16708,#16709,#16710,
#16711,#16712,#16713,#16714,#16715,#16716,#16717,#16718,#16719),
 .UNSPECIFIED.,.F.,.F.,(4,3,3,3,3,3,3,3,4),(38.8133028811071,38.9360263642056,
39.9343860145699,40.9327456649341,41.9311053152984,42.9294649656626,43.9278246160269,
44.9261842663911,45.0964881882867),.UNSPECIFIED.);
#1399=B_SPLINE_CURVE_WITH_KNOTS('',3,(#16724,#16725,#16726,#16727,#16728,
#16729,#16730,#16731,#16732,#16733,#16734,#16735,#16736,#16737,#16738,#16739,
#16740,#16741,#16742,#16743,#16744,#16745),.UNSPECIFIED.,.F.,.F.,(4,3,3,
3,3,3,3,4),(-54.358024206275,-53.8562759710472,-52.858937527139,-51.8615990832307,
-50.8642606393224,-49.8669221954141,-48.8695837515058,-48.0748388990954),
 .UNSPECIFIED.);
#1400=B_SPLINE_CURVE_WITH_KNOTS('',3,(#16746,#16747,#16748,#16749,#16750,
#16751,#16752,#16753,#16754,#16755,#16756,#16757,#16758,#16759,#16760,#16761,
#16762,#16763,#16764,#16765,#16766,#16767),.UNSPECIFIED.,.F.,.F.,(4,3,3,
3,3,3,3,4),(45.0964881882867,45.9245439167554,46.9229035671196,47.9212632174839,
48.9196228678481,49.9179825182124,50.9163421685766,51.3796734954663),
 .UNSPECIFIED.);
#1401=B_SPLINE_CURVE_WITH_KNOTS('',3,(#16772,#16773,#16774,#16775,#16776,
#16777,#16778,#16779,#16780,#16781,#16782,#16783,#16784,#16785,#16786,#16787,
#16788,#16789,#16790,#16791,#16792,#16793),.UNSPECIFIED.,.F.,.F.,(4,3,3,
3,3,3,3,4),(-60.6412095134546,-59.8403066344969,-58.8429681905886,-57.8456297466804,
-56.8482913027721,-55.8509528588638,-54.8536144149555,-54.358024206275),
 .UNSPECIFIED.);
#1402=B_SPLINE_CURVE_WITH_KNOTS('',3,(#16794,#16795,#16796,#16797,#16798,
#16799,#16800,#16801,#16802,#16803,#16804,#16805,#16806,#16807,#16808,#16809,
#16810,#16811,#16812,#16813,#16814,#16815),.UNSPECIFIED.,.F.,.F.,(4,3,3,
3,3,3,3,4),(51.3796734954663,51.9147018189409,52.9130614693051,53.9114211196693,
54.9097807700336,55.9081404203978,56.9065000707621,57.6628588026459),
 .UNSPECIFIED.);
#1403=B_SPLINE_CURVE_WITH_KNOTS('',3,(#16821,#16822,#16823,#16824,#16825,
#16826,#16827,#16828,#16829,#16830),.UNSPECIFIED.,.F.,.F.,(4,1,1,1,1,1,
1,4),(72.2566310325653,72.4530665975158,73.4504050414241,74.4477434853324,
75.4450819292407,76.4424203731489,77.4397588170572,78.4370972609655),
 .UNSPECIFIED.);
#1404=B_SPLINE_CURVE_WITH_KNOTS('',3,(#16833,#16834,#16835,#16836,#16837,
#16838,#16839,#16840),.UNSPECIFIED.,.F.,.F.,(4,1,1,1,1,4),(72.2566310325652,
73.2039641964158,74.2023238467801,75.2006834971443,76.1990431475085,77.1974027978728),
 .UNSPECIFIED.);
#1405=B_SPLINE_CURVE_WITH_KNOTS('',3,(#16845,#16846,#16847,#16848,#16849,
#16850,#16851,#16852,#16853,#16854),.UNSPECIFIED.,.F.,.F.,(4,1,1,1,1,1,
1,4),(65.9734457253856,66.4690359340661,67.4663743779744,68.4637128218827,
69.461051265791,70.4583897096992,71.4557281536075,72.2566310325653),
 .UNSPECIFIED.);
#1406=B_SPLINE_CURVE_WITH_KNOTS('',3,(#16855,#16856,#16857,#16858,#16859,
#16860,#16861,#16862,#16863,#16864,#16865),.UNSPECIFIED.,.F.,.F.,(4,1,1,
1,1,1,1,1,4),(65.9734457253856,66.2154466438661,67.2138062942303,68.2121659445946,
69.2105255949588,70.2088852453231,71.2072448956873,72.2056045460516,72.2566310325652),
 .UNSPECIFIED.);
#1407=B_SPLINE_CURVE_WITH_KNOTS('',3,(#16870,#16871,#16872,#16873,#16874,
#16875,#16876,#16877,#16878,#16879),.UNSPECIFIED.,.F.,.F.,(4,1,1,1,1,1,
1,4),(59.6902604182061,60.4850052706164,61.4823437145247,62.479682158433,
63.4770206023413,64.4743590462496,65.4716974901578,65.9734457253856),
 .UNSPECIFIED.);
#1408=B_SPLINE_CURVE_WITH_KNOTS('',3,(#16880,#16881,#16882,#16883,#16884,
#16885,#16886,#16887,#16888,#16889),.UNSPECIFIED.,.F.,.F.,(4,1,1,1,1,1,
1,4),(59.6902604182061,60.2252887416806,61.2236483920448,62.2220080424091,
63.2203676927733,64.2187273431376,65.2170869935018,65.9734457253856),
 .UNSPECIFIED.);
#1409=B_SPLINE_CURVE_WITH_KNOTS('',3,(#16894,#16895,#16896,#16897,#16898,
#16899,#16900,#16901,#16902,#16903,#16904),.UNSPECIFIED.,.F.,.F.,(4,1,1,
1,1,1,1,1,4),(53.4070751110265,53.5036361632585,54.5009746071667,55.498313051075,
56.4956514949833,57.4929899388916,58.4903283827999,59.4876668267081,59.6902604182061),
 .UNSPECIFIED.);
#1410=B_SPLINE_CURVE_WITH_KNOTS('',3,(#16905,#16906,#16907,#16908,#16909,
#16910,#16911,#16912,#16913,#16914),.UNSPECIFIED.,.F.,.F.,(4,1,1,1,1,1,
1,4),(53.4070751110265,54.2351308394951,55.2334904898594,56.2318501402236,
57.2302097905879,58.2285694409521,59.2269290913164,59.6902604182061),
 .UNSPECIFIED.);
#1411=B_SPLINE_CURVE_WITH_KNOTS('',3,(#16919,#16920,#16921,#16922,#16923,
#16924,#16925,#16926,#16927,#16928),.UNSPECIFIED.,.F.,.F.,(4,1,1,1,1,1,
1,4),(47.1238898038469,47.5196054998088,48.516943943717,49.5142823876253,
50.5116208315336,51.5089592754419,52.5062977193502,53.4070751110265),
 .UNSPECIFIED.);
#1412=B_SPLINE_CURVE_WITH_KNOTS('',3,(#16929,#16930,#16931,#16932,#16933,
#16934,#16935,#16936,#16937,#16938,#16939),.UNSPECIFIED.,.F.,.F.,(4,1,1,
1,1,1,1,1,4),(47.1238898038469,47.2466132869454,48.2449729373096,49.2433325876739,
50.2416922380381,51.2400518884024,52.2384115387666,53.2367711891309,53.4070751110265),
 .UNSPECIFIED.);
#1413=B_SPLINE_CURVE_WITH_KNOTS('',3,(#16944,#16945,#16946,#16947,#16948,
#16949,#16950,#16951,#16952,#16953),.UNSPECIFIED.,.F.,.F.,(4,1,1,1,1,1,
1,4),(40.8407044966673,41.5355748363591,42.5329132802674,43.5302517241756,
44.5275901680839,45.5249286119922,46.5222670559005,47.1238898038469),
 .UNSPECIFIED.);
#1414=B_SPLINE_CURVE_WITH_KNOTS('',3,(#16954,#16955,#16956,#16957,#16958,
#16959,#16960,#16961,#16962,#16963),.UNSPECIFIED.,.F.,.F.,(4,1,1,1,1,1,
1,4),(40.8407044966673,41.2564553847599,42.2548150351241,43.2531746854884,
44.2515343358526,45.2498939862169,46.2482536365811,47.1238898038469),
 .UNSPECIFIED.);
#1415=B_SPLINE_CURVE_WITH_KNOTS('',3,(#16968,#16969,#16970,#16971,#16972,
#16973,#16974,#16975,#16976,#16977),.UNSPECIFIED.,.F.,.F.,(4,1,1,1,1,1,
1,4),(34.5575191894877,35.5515441729094,36.5488826168177,37.5462210607259,
38.5435595046342,39.5408979485425,40.5382363924508,40.8407044966673),
 .UNSPECIFIED.);
#1416=B_SPLINE_CURVE_WITH_KNOTS('',3,(#16978,#16979,#16980,#16981,#16982,
#16983,#16984,#16985,#16986,#16987),.UNSPECIFIED.,.F.,.F.,(4,1,1,1,1,1,
1,4),(34.5575191894877,35.2662974825744,36.2646571329387,37.2630167833029,
38.2613764336672,39.2597360840314,40.2580957343957,40.8407044966673),
 .UNSPECIFIED.);
#1417=B_SPLINE_CURVE_WITH_KNOTS('',3,(#16992,#16993,#16994,#16995,#16996,
#16997,#16998,#16999,#17000,#17001,#17002),.UNSPECIFIED.,.F.,.F.,(4,1,1,
1,1,1,1,1,4),(28.2743338823081,28.5701750655514,29.5675135094597,30.564851953368,
31.5621903972762,32.5595288411845,33.5568672850928,34.5542057290011,34.5575191894877),
 .UNSPECIFIED.);
#1418=B_SPLINE_CURVE_WITH_KNOTS('',3,(#17003,#17004,#17005,#17006,#17007,
#17008,#17009,#17010,#17011,#17012,#17013),.UNSPECIFIED.,.F.,.F.,(4,1,1,
1,1,1,1,1,4),(28.2743338823081,28.2777799300247,29.2761395803889,30.2744992307532,
31.2728588811174,32.2712185314817,33.2695781818459,34.2679378322102,34.5575191894877),
 .UNSPECIFIED.);
#1419=B_SPLINE_CURVE_WITH_KNOTS('',3,(#17018,#17019,#17020,#17021,#17022,
#17023,#17024,#17025,#17026,#17027),.UNSPECIFIED.,.F.,.F.,(4,1,1,1,1,1,
1,4),(21.9911485751285,22.5861444021017,23.58348284601,24.5808212899183,
25.5781597338266,26.5754981777348,27.5728366216431,28.2743338823081),
 .UNSPECIFIED.);
#1420=B_SPLINE_CURVE_WITH_KNOTS('',3,(#17028,#17029,#17030,#17031,#17032,
#17033,#17034,#17035,#17036,#17037),.UNSPECIFIED.,.F.,.F.,(4,1,1,1,1,1,
1,4),(21.9911485751285,22.2876220278392,23.2859816782034,24.2843413285677,
25.2827009789319,26.2810606292962,27.2794202796604,28.2743338823081),
 .UNSPECIFIED.);
#1421=B_SPLINE_CURVE_WITH_KNOTS('',3,(#17042,#17043,#17044,#17045,#17046,
#17047,#17048,#17049,#17050,#17051),.UNSPECIFIED.,.F.,.F.,(4,1,1,1,1,1,
1,4),(15.7079632679489,16.602113738652,17.5994521825603,18.5967906264686,
19.5941290703769,20.5914675142851,21.5888059581934,21.9911485751285),
 .UNSPECIFIED.);
#1422=B_SPLINE_CURVE_WITH_KNOTS('',3,(#17052,#17053,#17054,#17055,#17056,
#17057,#17058,#17059,#17060,#17061),.UNSPECIFIED.,.F.,.F.,(4,1,1,1,1,1,
1,4),(15.7079632679489,16.2974641256537,17.295823776018,18.2941834263822,
19.2925430767465,20.2909027271107,21.289262377475,21.9911485751285),
 .UNSPECIFIED.);
#1423=B_SPLINE_CURVE_WITH_KNOTS('',3,(#17064,#17065,#17066,#17067,#17068,
#17069,#17070,#17071,#17072,#17073,#17074,#17075,#17076,#17077,#17078,#17079,
#17080,#17081,#17082,#17083,#17084,#17085,#17086,#17087,#17088,#17089,#17090,
#17091,#17092,#17093,#17094,#17095,#17096,#17097,#17098,#17099,#17100,#17101,
#17102,#17103,#17104,#17105,#17106,#17107,#17108,#17109,#17110,#17111,#17112,
#17113,#17114,#17115,#17116,#17117,#17118,#17119,#17120,#17121,#17122,#17123,
#17124,#17125,#17126,#17127,#17128,#17129,#17130,#17131,#17132,#17133,#17134,
#17135,#17136,#17137,#17138,#17139,#17140,#17141,#17142,#17143,#17144,#17145,
#17146,#17147,#17148,#17149,#17150,#17151,#17152,#17153,#17154,#17155,#17156,
#17157,#17158,#17159,#17160,#17161,#17162,#17163,#17164,#17165,#17166,#17167,
#17168,#17169,#17170,#17171,#17172,#17173,#17174,#17175,#17176,#17177,#17178,
#17179,#17180,#17181,#17182,#17183,#17184,#17185,#17186,#17187,#17188,#17189,
#17190,#17191,#17192,#17193,#17194,#17195,#17196,#17197,#17198,#17199,#17200,
#17201,#17202,#17203,#17204,#17205,#17206,#17207,#17208,#17209,#17210,#17211,
#17212,#17213,#17214,#17215,#17216,#17217,#17218,#17219,#17220,#17221,#17222,
#17223,#17224,#17225,#17226,#17227,#17228,#17229,#17230,#17231,#17232,#17233,
#17234,#17235,#17236,#17237,#17238,#17239,#17240,#17241,#17242,#17243,#17244,
#17245,#17246,#17247,#17248,#17249,#17250,#17251,#17252,#17253,#17254,#17255,
#17256,#17257,#17258,#17259,#17260,#17261,#17262,#17263,#17264,#17265,#17266,
#17267,#17268),.UNSPECIFIED.,.F.,.F.,(4,3,3,3,3,3,3,3,3,3,3,3,3,3,3,3,3,
3,3,3,3,3,3,3,3,3,3,3,3,3,3,3,3,3,3,3,3,3,3,3,3,3,3,3,3,3,3,3,3,3,3,3,3,
3,3,3,3,3,3,3,3,3,3,3,3,3,3,3,4),(-0.996917990983889,-0.978871820698626,
-0.961104366684017,-0.951552920986235,-0.947856438601261,-0.928927311919591,
-0.909844934708151,-0.904827747876617,-0.901690020918146,-0.882383426909664,
-0.863197144412726,-0.849964666497242,-0.841946217765742,-0.838653066670214,
-0.836732188581758,-0.818195847210497,-0.79884286378821,-0.782668226932182,
-0.778162385717433,-0.774287931072979,-0.754720517493441,-0.734912656248282,
-0.718545934421209,-0.712508687338266,-0.709097549624951,-0.689177599037007,
-0.66944576893999,-0.649768871196005,-0.645300371314176,-0.641533261094732,
-0.621745212512907,-0.601563770435519,-0.588280416256018,-0.579851467607475,
-0.575105400436484,-0.55460765219522,-0.534203727151442,-0.514750332075477,
-0.510181591792683,-0.506682086087755,-0.495296936999511,-0.475415657124971,
-0.455258237398922,-0.446439366268775,-0.440745412953617,-0.437134753004049,
-0.41645257608894,-0.395479514073081,-0.375148710383956,-0.368821709024976,
-0.365366889657485,-0.344172462410384,-0.323356461419818,-0.31415629931658,
-0.303019600034791,-0.297245219492413,-0.293778204123757,-0.272935156968737,
-0.251638706464901,-0.237180007007782,-0.228159672465448,-0.224715742096491,
-0.221072456791868,-0.199410898099475,-0.17780203126093,-0.156885571034439,
-0.151911241963545,-0.148372189075213,-0.135969110807948),.UNSPECIFIED.);
#1424=B_SPLINE_CURVE_WITH_KNOTS('',3,(#17270,#17271,#17272,#17273,#17274,
#17275,#17276,#17277,#17278,#17279,#17280,#17281,#17282,#17283,#17284,#17285,
#17286,#17287,#17288,#17289,#17290,#17291,#17292,#17293,#17294,#17295,#17296,
#17297,#17298,#17299,#17300,#17301,#17302,#17303,#17304,#17305,#17306,#17307,
#17308,#17309,#17310,#17311,#17312,#17313,#17314,#17315,#17316,#17317,#17318,
#17319,#17320,#17321,#17322,#17323,#17324,#17325,#17326,#17327),
 .UNSPECIFIED.,.F.,.F.,(4,3,3,3,3,3,3,3,3,3,3,3,3,3,3,3,3,3,3,4),(-0.271362855059846,
-0.249815149227379,-0.228817911637578,-0.214757147690894,-0.202696405081427,
-0.199258885355278,-0.179079500439592,-0.172574855850844,-0.151002998869488,
-0.132127624010802,-0.128545226638174,-0.108660379749781,-0.0889046558653028,
-0.0695674270863146,-0.0643977980835871,-0.0611874131352371,-0.042433397437552,
-0.0240016538661123,-0.00610725636958426,0.),.UNSPECIFIED.);
#1425=B_SPLINE_CURVE_WITH_KNOTS('',3,(#17330,#17331,#17332,#17333,#17334,
#17335,#17336,#17337,#17338,#17339,#17340,#17341,#17342,#17343,#17344,#17345,
#17346,#17347,#17348,#17349,#17350,#17351,#17352,#17353,#17354,#17355,#17356,
#17357),.UNSPECIFIED.,.F.,.F.,(4,3,3,3,3,3,3,3,3,4),(-0.135969110807948,
-0.126188073854222,-0.104892740575823,-0.0831670570417323,-0.0779384685470277,
-0.0734086019617295,-0.0516285578143609,-0.0295399653803274,-0.00752416693119264,
0.),.UNSPECIFIED.);
#1426=B_SPLINE_CURVE_WITH_KNOTS('',3,(#17642,#17643,#17644,#17645,#17646,
#17647,#17648,#17649),.UNSPECIFIED.,.F.,.F.,(4,1,1,1,1,4),(11.6154215191106,
12.6127599630189,13.6100984069272,14.6074368508354,15.6047752947437,15.7079632679489),
 .UNSPECIFIED.);
#1427=B_SPLINE_CURVE_WITH_KNOTS('',3,(#17650,#17651,#17652,#17653,#17654,
#17655,#17656,#17657,#17658,#17659,#17660,#17661,#17662,#17663,#17664,#17665,
#17666,#17667,#17668,#17669,#17670,#17671,#17672,#17673,#17674,#17675,#17676,
#17677,#17678,#17679,#17680,#17681,#17682,#17683,#17684,#17685,#17686,#17687,
#17688,#17689,#17690,#17691,#17692,#17693,#17694,#17695,#17696,#17697,#17698,
#17699,#17700,#17701,#17702,#17703,#17704,#17705,#17706,#17707,#17708,#17709,
#17710,#17711,#17712,#17713,#17714,#17715,#17716,#17717,#17718,#17719,#17720,
#17721,#17722,#17723,#17724,#17725,#17726,#17727,#17728,#17729,#17730,#17731,
#17732,#17733,#17734),.UNSPECIFIED.,.F.,.F.,(4,3,3,3,3,3,3,3,3,3,3,3,3,
3,3,3,3,3,3,3,3,3,3,3,3,3,3,3,4),(-0.364629307890661,-0.350886771084415,
-0.329297510939725,-0.318979842765136,-0.313748856729508,-0.309367238941102,
-0.288044972781349,-0.272811108278258,-0.264009728102714,-0.260298972601032,
-0.239567880035138,-0.219347617431434,-0.206054227262732,-0.194878207820902,
-0.191399429390758,-0.17181371271556,-0.166174056756627,-0.145402299662048,
-0.12670765132229,-0.123381127587156,-0.103926762733045,-0.0845494608218094,
-0.0655688723802368,-0.0621691825638593,-0.0589309125894093,-0.0403408647045067,
-0.0220852216194749,-0.00441218938162483,0.),.UNSPECIFIED.);
#1428=B_SPLINE_CURVE_WITH_KNOTS('',3,(#17735,#17736,#17737,#17738,#17739,
#17740,#17741,#17742,#17743,#17744,#17745,#17746,#17747,#17748,#17749,#17750,
#17751,#17752,#17753),.UNSPECIFIED.,.F.,.F.,(4,3,3,3,3,3,4),(-65.3098882395457,
-64.8269988540384,-63.8296604101301,-62.8323219662218,-61.8349835223135,
-60.8376450784052,-60.6412095134546),.UNSPECIFIED.);
#1429=B_SPLINE_CURVE_WITH_KNOTS('',3,(#17756,#17757,#17758,#17759,#17760,
#17761,#17762,#17763,#17764),.UNSPECIFIED.,.F.,.F.,(4,1,1,1,1,1,4),(10.3757270560179,
11.3056658738325,12.3040255241967,13.302385174561,14.3007448249252,15.2991044752895,
15.7079632679489),.UNSPECIFIED.);
#1430=B_SPLINE_CURVE_WITH_KNOTS('',3,(#18054,#18055,#18056,#18057,#18058,
#18059,#18060,#18061,#18062,#18063,#18064,#18065,#18066,#18067,#18068,#18069,
#18070,#18071,#18072,#18073,#18074,#18075),.UNSPECIFIED.,.F.,.F.,(4,3,3,
3,3,3,3,4),(57.6628588026459,57.9048597211263,58.9032193714906,59.9015790218548,
60.8999386722191,61.8982983225833,62.8966579729476,63.2447481062677),
 .UNSPECIFIED.);
#1431=B_SPLINE_CURVE_WITH_KNOTS('',3,(#18076,#18077,#18078,#18079,#18080,
#18081,#18082,#18083,#18084,#18085,#18086,#18087,#18088,#18089,#18090,#18091,
#18092,#18093,#18094,#18095,#18096,#18097,#18098,#18099,#18100,#18101,#18102,
#18103,#18104,#18105,#18106,#18107,#18108,#18109,#18110,#18111,#18112,#18113,
#18114,#18115,#18116,#18117,#18118,#18119,#18120,#18121,#18122,#18123,#18124,
#18125,#18126,#18127,#18128,#18129,#18130,#18131,#18132,#18133,#18134,#18135,
#18136,#18137,#18138,#18139,#18140,#18141,#18142,#18143,#18144,#18145,#18146,
#18147,#18148,#18149,#18150,#18151,#18152,#18153,#18154,#18155,#18156,#18157),
 .UNSPECIFIED.,.F.,.F.,(4,3,3,3,3,3,3,3,3,3,3,3,3,3,3,3,3,3,3,3,3,3,3,3,
3,3,3,4),(-0.366397579005847,-0.355573362530754,-0.337605442405704,-0.327398200425482,
-0.321620335202968,-0.30281021010297,-0.288367976755365,-0.281197910953663,
-0.277581602535663,-0.258139779174731,-0.23832225991534,-0.225559780767037,
-0.21845666374658,-0.214865898441521,-0.194435927724086,-0.187272343322128,
-0.167568574984456,-0.146399230996079,-0.142991450501546,-0.122489503287978,
-0.101565610408655,-0.0804999660718792,-0.0757146540182571,-0.0722132271210984,
-0.0505693460362938,-0.0288755213118303,-0.00764564704115539,0.),
 .UNSPECIFIED.);
#1432=B_SPLINE_CURVE_WITH_KNOTS('',3,(#18211,#18212,#18213,#18214,#18215,
#18216,#18217,#18218,#18219,#18220),.UNSPECIFIED.,.F.,.F.,(4,3,3,4),(-4.09293042013066,
-3.96748245563351,-2.97561184172513,-2.06863817490915),.UNSPECIFIED.);
#1433=B_SPLINE_CURVE_WITH_KNOTS('',3,(#18223,#18224,#18225,#18226,#18227,
#18228,#18229),.UNSPECIFIED.,.F.,.F.,(4,3,4),(0.,0.992711177740983,1.1173004083682),
 .UNSPECIFIED.);
#1434=B_SPLINE_CURVE_WITH_KNOTS('',3,(#18234,#18235,#18236,#18237,#18238,
#18239,#18240,#18241,#18242,#18243,#18244,#18245,#18246,#18247,#18248,#18249,
#18250,#18251,#18252,#18253,#18254,#18255),.UNSPECIFIED.,.F.,.F.,(4,3,3,
3,3,3,3,4),(-10.3761157273102,-9.91870613908378,-8.9268355251754,-7.93496491126702,
-6.94309429735864,-5.95122368345026,-4.95935306954189,-4.09293042013066),
 .UNSPECIFIED.);
#1435=B_SPLINE_CURVE_WITH_KNOTS('',3,(#18256,#18257,#18258,#18259,#18260,
#18261,#18262,#18263,#18264,#18265,#18266,#18267,#18268,#18269,#18270,#18271,
#18272,#18273,#18274,#18275,#18276,#18277),.UNSPECIFIED.,.F.,.F.,(4,3,3,
3,3,3,3,4),(1.1173004083682,1.98542235548196,2.97813353322293,3.97084471096391,
4.96355588870488,5.95626706644586,6.94897824418683,7.40048571554779),
 .UNSPECIFIED.);
#1436=B_SPLINE_CURVE_WITH_KNOTS('',3,(#18282,#18283,#18284,#18285,#18286,
#18287,#18288,#18289,#18290,#18291,#18292,#18293,#18294,#18295,#18296,#18297,
#18298,#18299,#18300,#18301,#18302,#18303),.UNSPECIFIED.,.F.,.F.,(4,3,3,
3,3,3,3,4),(-16.6593010344898,-15.869929822534,-14.8780592086257,-13.8861885947173,
-12.8943179808089,-11.9024473669005,-10.9105767529922,-10.3761157273102),
 .UNSPECIFIED.);
#1437=B_SPLINE_CURVE_WITH_KNOTS('',3,(#18304,#18305,#18306,#18307,#18308,
#18309,#18310,#18311,#18312,#18313,#18314,#18315,#18316,#18317,#18318,#18319,
#18320,#18321,#18322,#18323,#18324,#18325),.UNSPECIFIED.,.F.,.F.,(4,3,3,
3,3,3,3,4),(7.40048571554779,7.94168942192781,8.93440059966879,9.92711177740977,
10.9198229551507,11.9125341328917,12.9052453106327,13.6836710227274),
 .UNSPECIFIED.);
#1438=B_SPLINE_CURVE_WITH_KNOTS('',3,(#18330,#18331,#18332,#18333,#18334,
#18335,#18336,#18337,#18338,#18339,#18340,#18341,#18342,#18343,#18344,#18345,
#18346,#18347,#18348,#18349,#18350,#18351,#18352,#18353,#18354),
 .UNSPECIFIED.,.F.,.F.,(4,3,3,3,3,3,3,3,4),(-22.9424863416694,-22.8130241198927,
-21.8211535059843,-20.8292828920759,-19.8374122781676,-18.8455416642592,
-17.8536710503508,-16.8618004364424,-16.6593010344898),.UNSPECIFIED.);
#1439=B_SPLINE_CURVE_WITH_KNOTS('',3,(#18355,#18356,#18357,#18358,#18359,
#18360,#18361,#18362,#18363,#18364,#18365,#18366,#18367,#18368,#18369,#18370,
#18371,#18372,#18373,#18374,#18375,#18376,#18377,#18378,#18379),
 .UNSPECIFIED.,.F.,.F.,(4,3,3,3,3,3,3,3,4),(13.6836710227274,13.8979564883737,
14.8906676661147,15.8833788438556,16.8760900215966,17.8688011993376,18.8615123770786,
19.8542235548195,19.966856329907),.UNSPECIFIED.);
#1440=B_SPLINE_CURVE_WITH_KNOTS('',3,(#18384,#18385,#18386,#18387,#18388,
#18389,#18390,#18391,#18392,#18393,#18394,#18395,#18396,#18397,#18398,#18399,
#18400,#18401,#18402,#18403,#18404,#18405),.UNSPECIFIED.,.F.,.F.,(4,3,3,
3,3,3,3,4),(-29.225671648849,-28.764247803343,-27.7723771894346,-26.7805065755262,
-25.7886359616178,-24.7967653477094,-23.8048947338011,-22.9424863416694),
 .UNSPECIFIED.);
#1441=B_SPLINE_CURVE_WITH_KNOTS('',3,(#18406,#18407,#18408,#18409,#18410,
#18411,#18412,#18413,#18414,#18415,#18416,#18417,#18418,#18419,#18420,#18421,
#18422,#18423,#18424,#18425,#18426,#18427),.UNSPECIFIED.,.F.,.F.,(4,3,3,
3,3,3,3,4),(19.966856329907,20.8469347325605,21.8396459103015,22.8323570880425,
23.8250682657834,24.8177794435244,25.8104906212654,26.2500416370865),
 .UNSPECIFIED.);
#1442=B_SPLINE_CURVE_WITH_KNOTS('',3,(#18432,#18433,#18434,#18435,#18436,
#18437,#18438,#18439,#18440,#18441,#18442,#18443,#18444,#18445,#18446,#18447,
#18448,#18449,#18450,#18451,#18452,#18453),.UNSPECIFIED.,.F.,.F.,(4,3,3,
3,3,3,3,4),(-35.5088569560286,-34.7154714867932,-33.7236008728848,-32.7317302589765,
-31.7398596450681,-30.7479890311597,-29.7561184172513,-29.225671648849),
 .UNSPECIFIED.);
#1443=B_SPLINE_CURVE_WITH_KNOTS('',3,(#18454,#18455,#18456,#18457,#18458,
#18459,#18460,#18461,#18462,#18463,#18464,#18465,#18466,#18467,#18468,#18469,
#18470,#18471,#18472,#18473,#18474,#18475),.UNSPECIFIED.,.F.,.F.,(4,3,3,
3,3,3,3,4),(26.2500416370865,26.8032017990064,27.7959129767474,28.7886241544883,
29.7813353322293,30.7740465099703,31.7667576877113,32.5332269442661),
 .UNSPECIFIED.);
#1444=B_SPLINE_CURVE_WITH_KNOTS('',3,(#18480,#18481,#18482,#18483,#18484,
#18485,#18486,#18487,#18488,#18489,#18490,#18491,#18492,#18493,#18494,#18495,
#18496,#18497,#18498,#18499,#18500,#18501,#18502,#18503,#18504),
 .UNSPECIFIED.,.F.,.F.,(4,3,3,3,3,3,3,3,4),(-41.7920422632082,-41.6585657841519,
-40.6666951702435,-39.6748245563351,-38.6829539424267,-37.6910833285184,
-36.69921271461,-35.7073421007016,-35.5088569560286),.UNSPECIFIED.);
#1445=B_SPLINE_CURVE_WITH_KNOTS('',3,(#18505,#18506,#18507,#18508,#18509,
#18510,#18511,#18512,#18513,#18514,#18515,#18516,#18517,#18518,#18519,#18520,
#18521,#18522,#18523,#18524,#18525,#18526,#18527,#18528,#18529),
 .UNSPECIFIED.,.F.,.F.,(4,3,3,3,3,3,3,3,4),(32.5332269442661,32.7594688654522,
33.7521800431932,34.7448912209342,35.7376023986752,36.7303135764161,37.7230247541571,
38.7157359318981,38.8164122514457),.UNSPECIFIED.);
#1446=B_SPLINE_CURVE_WITH_KNOTS('',3,(#18534,#18535,#18536,#18537,#18538,
#18539,#18540,#18541,#18542,#18543,#18544,#18545,#18546,#18547,#18548,#18549,
#18550,#18551,#18552,#18553,#18554,#18555),.UNSPECIFIED.,.F.,.F.,(4,3,3,
3,3,3,3,4),(-48.0752275703878,-47.6097894676021,-46.6179188536938,-45.6260482397854,
-44.634177625877,-43.6423070119686,-42.6504363980602,-41.7920422632082),
 .UNSPECIFIED.);
#1447=B_SPLINE_CURVE_WITH_KNOTS('',3,(#18556,#18557,#18558,#18559,#18560,
#18561,#18562,#18563,#18564,#18565,#18566,#18567,#18568,#18569,#18570,#18571,
#18572,#18573,#18574,#18575,#18576,#18577),.UNSPECIFIED.,.F.,.F.,(4,3,3,
3,3,3,3,4),(38.8164122514457,39.7084471096391,40.7011582873801,41.693869465121,
42.686580642862,43.679291820603,44.672002998344,45.0995975586253),
 .UNSPECIFIED.);
#1448=B_SPLINE_CURVE_WITH_KNOTS('',3,(#18582,#18583,#18584,#18585,#18586,
#18587,#18588,#18589,#18590,#18591,#18592,#18593,#18594,#18595,#18596,#18597,
#18598,#18599,#18600,#18601,#18602,#18603),.UNSPECIFIED.,.F.,.F.,(4,3,3,
3,3,3,3,4),(-54.3584128775674,-53.5610131510524,-52.569142537144,-51.5772719232356,
-50.5854013093273,-49.5935306954189,-48.6016600815105,-48.0752275703878),
 .UNSPECIFIED.);
#1449=B_SPLINE_CURVE_WITH_KNOTS('',3,(#18604,#18605,#18606,#18607,#18608,
#18609,#18610,#18611,#18612,#18613,#18614,#18615,#18616,#18617,#18618,#18619,
#18620,#18621,#18622,#18623,#18624,#18625),.UNSPECIFIED.,.F.,.F.,(4,3,3,
3,3,3,3,4),(45.0995975586253,45.6647141760849,46.6574253538259,47.6501365315669,
48.6428477093079,49.6355588870488,50.6282700647898,51.3827828658049),
 .UNSPECIFIED.);
#1450=B_SPLINE_CURVE_WITH_KNOTS('',3,(#18630,#18631,#18632,#18633,#18634,
#18635,#18636,#18637,#18638,#18639,#18640,#18641,#18642,#18643,#18644,#18645,
#18646,#18647,#18648,#18649,#18650,#18651,#18652,#18653,#18654),
 .UNSPECIFIED.,.F.,.F.,(4,3,3,3,3,3,3,3,4),(-60.641598184747,-60.5041074484111,
-59.5122368345027,-58.5203662205943,-57.5284956066859,-56.5366249927775,
-55.5447543788692,-54.5528837649608,-54.3584128775674),.UNSPECIFIED.);
#1451=B_SPLINE_CURVE_WITH_KNOTS('',3,(#18655,#18656,#18657,#18658,#18659,
#18660,#18661,#18662,#18663,#18664,#18665,#18666,#18667,#18668,#18669,#18670,
#18671,#18672,#18673,#18674,#18675,#18676,#18677,#18678,#18679),
 .UNSPECIFIED.,.F.,.F.,(4,3,3,3,3,3,3,3,4),(51.3827828658049,51.6209812425308,
52.6136924202718,53.6064035980127,54.5991147757537,55.5918259534947,56.5845371312357,
57.5772483089767,57.6659681729845),.UNSPECIFIED.);
#1452=B_SPLINE_CURVE_WITH_KNOTS('',3,(#18684,#18685,#18686,#18687,#18688,
#18689,#18690,#18691,#18692,#18693,#18694,#18695,#18696,#18697,#18698,#18699,
#18700,#18701,#18702,#18703,#18704,#18705),.UNSPECIFIED.,.F.,.F.,(4,3,3,
3,3,3,3,4),(-66.9247834919266,-66.4553311318613,-65.4634605179529,-64.4715899040445,
-63.4797192901362,-62.4878486762278,-61.4959780623194,-60.641598184747),
 .UNSPECIFIED.);
#1453=B_SPLINE_CURVE_WITH_KNOTS('',3,(#18706,#18707,#18708,#18709,#18710,
#18711,#18712,#18713,#18714,#18715,#18716,#18717,#18718,#18719,#18720,#18721,
#18722,#18723,#18724,#18725,#18726,#18727),.UNSPECIFIED.,.F.,.F.,(4,3,3,
3,3,3,3,4),(57.6659681729845,58.5699594867177,59.5626706644586,60.5553818421996,
61.5480930199406,62.5408041976816,63.5335153754225,63.9491534801641),
 .UNSPECIFIED.);
#1454=B_SPLINE_CURVE_WITH_KNOTS('',3,(#18732,#18733,#18734,#18735,#18736,
#18737,#18738,#18739,#18740,#18741,#18742,#18743,#18744,#18745,#18746,#18747,
#18748,#18749,#18750,#18751,#18752,#18753),.UNSPECIFIED.,.F.,.F.,(4,3,3,
3,3,3,3,4),(-73.2079687991062,-72.4065548153116,-71.4146842014032,-70.4228135874948,
-69.4309429735864,-68.4390723596781,-67.4472017457697,-66.9247834919266),
 .UNSPECIFIED.);
#1455=B_SPLINE_CURVE_WITH_KNOTS('',3,(#18754,#18755,#18756,#18757,#18758,
#18759,#18760,#18761,#18762,#18763,#18764,#18765,#18766,#18767,#18768,#18769,
#18770,#18771,#18772,#18773,#18774,#18775),.UNSPECIFIED.,.F.,.F.,(4,3,3,
3,3,3,3,4),(63.9491534801641,64.5262265531635,65.5189377309045,66.5116489086455,
67.5043600863864,68.4970712641274,69.4897824418684,70.2323387873437),
 .UNSPECIFIED.);
#1456=B_SPLINE_CURVE_WITH_KNOTS('',3,(#18780,#18781,#18782,#18783,#18784,
#18785,#18786,#18787,#18788,#18789,#18790,#18791,#18792,#18793,#18794,#18795,
#18796,#18797,#18798,#18799,#18800,#18801,#18802,#18803,#18804),
 .UNSPECIFIED.,.F.,.F.,(4,3,3,3,3,3,3,3,4),(-79.4911541062857,-79.3496491126702,
-78.3577784987618,-77.3659078848535,-76.3740372709451,-75.3821666570367,
-74.3902960431283,-73.3984254292199,-73.2079687991062),.UNSPECIFIED.);
#1457=B_SPLINE_CURVE_WITH_KNOTS('',3,(#18805,#18806,#18807,#18808,#18809,
#18810,#18811,#18812,#18813,#18814,#18815,#18816,#18817,#18818,#18819,#18820,
#18821,#18822,#18823,#18824,#18825,#18826,#18827,#18828,#18829),
 .UNSPECIFIED.,.F.,.F.,(4,3,3,3,3,3,3,3,4),(70.2323387873437,70.4824936196094,
71.4752047973503,72.4679159750913,73.4606271528323,74.4533383305733,75.4460495083142,
76.4387606860552,76.5155240945233),.UNSPECIFIED.);
#1458=B_SPLINE_CURVE_WITH_KNOTS('',3,(#18834,#18835,#18836,#18837,#18838,
#18839,#18840,#18841,#18842,#18843,#18844,#18845,#18846,#18847,#18848,#18849,
#18850,#18851,#18852,#18853,#18854,#18855),.UNSPECIFIED.,.F.,.F.,(4,3,3,
3,3,3,3,4),(-85.7743394134653,-85.3008727961205,-84.3090021822121,-83.3171315683037,
-82.3252609543953,-81.333390340487,-80.3415197265786,-79.4911541062857),
 .UNSPECIFIED.);
#1459=B_SPLINE_CURVE_WITH_KNOTS('',3,(#18856,#18857,#18858,#18859,#18860,
#18861,#18862,#18863,#18864,#18865,#18866,#18867,#18868,#18869,#18870,#18871,
#18872,#18873,#18874,#18875,#18876,#18877),.UNSPECIFIED.,.F.,.F.,(4,3,3,
3,3,3,3,4),(76.5155240945233,77.4314718637962,78.4241830415372,79.4168942192782,
80.4096053970191,81.4023165747601,82.3950277525011,82.7987094017029),
 .UNSPECIFIED.);
#1460=B_SPLINE_CURVE_WITH_KNOTS('',3,(#18882,#18883,#18884,#18885,#18886,
#18887,#18888,#18889,#18890,#18891,#18892,#18893,#18894,#18895,#18896,#18897,
#18898,#18899,#18900,#18901,#18902,#18903),.UNSPECIFIED.,.F.,.F.,(4,3,3,
3,3,3,3,4),(-92.0575247206449,-91.2520964795708,-90.2602258656624,-89.268355251754,
-88.2764846378456,-87.2846140239373,-86.2927434100289,-85.7743394134653),
 .UNSPECIFIED.);
#1461=B_SPLINE_CURVE_WITH_KNOTS('',3,(#18904,#18905,#18906,#18907,#18908,
#18909,#18910,#18911,#18912,#18913,#18914,#18915,#18916,#18917,#18918,#18919,
#18920,#18921,#18922,#18923,#18924,#18925),.UNSPECIFIED.,.F.,.F.,(4,3,3,
3,3,3,3,4),(82.7987094017029,83.3877389302421,84.380450107983,85.373161285724,
86.365872463465,87.358583641206,88.351294818947,89.0818947088825),
 .UNSPECIFIED.);
#1462=B_SPLINE_CURVE_WITH_KNOTS('',3,(#18931,#18932,#18933,#18934,#18935,
#18936,#18937,#18938,#18939,#18940),.UNSPECIFIED.,.F.,.F.,(4,1,1,1,1,1,
1,4),(103.672557568463,103.858999941297,104.850870555206,105.842741169114,
106.834611783022,107.826482396931,108.818353010839,109.810223624748),
 .UNSPECIFIED.);
#1463=B_SPLINE_CURVE_WITH_KNOTS('',3,(#18943,#18944,#18945,#18946,#18947,
#18948,#18949,#18950),.UNSPECIFIED.,.F.,.F.,(4,1,1,1,1,4),(103.672557568463,
104.600461793276,105.593172971017,106.585884148758,107.578595326499,108.57130650424),
 .UNSPECIFIED.);
#1464=B_SPLINE_CURVE_WITH_KNOTS('',3,(#18955,#18956,#18957,#18958,#18959,
#18960,#18961,#18962,#18963,#18964),.UNSPECIFIED.,.F.,.F.,(4,1,1,1,1,1,
1,4),(97.3893722612836,97.9077762578471,98.8996468717555,99.8915174856638,
100.883388099572,101.875258713481,102.867129327389,103.672557568463),
 .UNSPECIFIED.);
#1465=B_SPLINE_CURVE_WITH_KNOTS('',3,(#18965,#18966,#18967,#18968,#18969,
#18970,#18971,#18972,#18973,#18974,#18975),.UNSPECIFIED.,.F.,.F.,(4,1,1,
1,1,1,1,1,4),(97.3893722612836,97.6514835490889,98.6441947268299,99.6369059045709,
100.629617082312,101.622328260053,102.615039437794,103.607750615535,103.672557568463),
 .UNSPECIFIED.);
#1466=B_SPLINE_CURVE_WITH_KNOTS('',3,(#18980,#18981,#18982,#18983,#18984,
#18985,#18986,#18987,#18988,#18989),.UNSPECIFIED.,.F.,.F.,(4,1,1,1,1,1,
1,4),(91.106186954104,91.9565525743968,92.9484231883052,93.9402938022136,
94.9321644161219,95.9240350300303,96.9159056439387,97.3893722612836),
 .UNSPECIFIED.);
#1467=B_SPLINE_CURVE_WITH_KNOTS('',3,(#18990,#18991,#18992,#18993,#18994,
#18995,#18996,#18997,#18998,#18999),.UNSPECIFIED.,.F.,.F.,(4,1,1,1,1,1,
1,4),(91.106186954104,91.6952164826431,92.687927660384,93.680638838125,
94.673350015866,95.666061193607,96.658772371348,97.3893722612836),
 .UNSPECIFIED.);
#1468=B_SPLINE_CURVE_WITH_KNOTS('',3,(#19004,#19005,#19006,#19007,#19008,
#19009,#19010,#19011,#19012,#19013,#19014),.UNSPECIFIED.,.F.,.F.,(4,1,1,
1,1,1,1,1,4),(84.8230016469244,85.0134582770382,86.0053288909465,86.9971995048549,
87.9890701187633,88.9809407326717,89.9728113465801,90.9646819604884,91.106186954104),
 .UNSPECIFIED.);
#1469=B_SPLINE_CURVE_WITH_KNOTS('',3,(#19015,#19016,#19017,#19018,#19019,
#19020,#19021,#19022,#19023,#19024),.UNSPECIFIED.,.F.,.F.,(4,1,1,1,1,1,
1,4),(84.8230016469244,85.7389494161972,86.7316605939382,87.7243717716792,
88.7170829494201,89.7097941271611,90.7025053049021,91.106186954104),
 .UNSPECIFIED.);
#1470=B_SPLINE_CURVE_WITH_KNOTS('',3,(#19029,#19030,#19031,#19032,#19033,
#19034,#19035,#19036,#19037,#19038),.UNSPECIFIED.,.F.,.F.,(4,1,1,1,1,1,
1,4),(78.5398163397448,79.0622345935879,80.0541052074963,81.0459758214047,
82.037846435313,83.0297170492214,84.0215876631298,84.8230016469244),
 .UNSPECIFIED.);
#1471=B_SPLINE_CURVE_WITH_KNOTS('',3,(#19039,#19040,#19041,#19042,#19043,
#19044,#19045,#19046,#19047,#19048,#19049),.UNSPECIFIED.,.F.,.F.,(4,1,1,
1,1,1,1,1,4),(78.5398163397448,78.7899711720104,79.7826823497514,80.7753935274923,
81.7681047052333,82.7608158829743,83.7535270607153,84.7462382384562,84.8230016469244),
 .UNSPECIFIED.);
#1472=B_SPLINE_CURVE_WITH_KNOTS('',3,(#19054,#19055,#19056,#19057,#19058,
#19059,#19060,#19061,#19062,#19063),.UNSPECIFIED.,.F.,.F.,(4,1,1,1,1,1,
1,4),(72.2566310325652,73.1110109101376,74.102881524046,75.0947521379544,
76.0866227518628,77.0784933657711,78.0703639796795,78.5398163397448),
 .UNSPECIFIED.);
#1473=B_SPLINE_CURVE_WITH_KNOTS('',3,(#19064,#19065,#19066,#19067,#19068,
#19069,#19070,#19071,#19072,#19073),.UNSPECIFIED.,.F.,.F.,(4,1,1,1,1,1,
1,4),(72.2566310325652,72.8337041055645,73.8264152833055,74.8191264610465,
75.8118376387874,76.8045488165284,77.7972599942694,78.5398163397448),
 .UNSPECIFIED.);
#1474=B_SPLINE_CURVE_WITH_KNOTS('',3,(#19078,#19079,#19080,#19081,#19082,
#19083,#19084,#19085,#19086,#19087,#19088),.UNSPECIFIED.,.F.,.F.,(4,1,1,
1,1,1,1,1,4),(65.9734457253856,66.167916612779,67.1597872266874,68.1516578405957,
69.1435284545041,70.1353990684125,71.1272696823209,72.1191402962293,72.2566310325652),
 .UNSPECIFIED.);
#1475=B_SPLINE_CURVE_WITH_KNOTS('',3,(#19089,#19090,#19091,#19092,#19093,
#19094,#19095,#19096,#19097,#19098),.UNSPECIFIED.,.F.,.F.,(4,1,1,1,1,1,
1,4),(65.9734457253856,66.8774370391187,67.8701482168596,68.8628593946006,
69.8555705723416,70.8482817500825,71.8409929278235,72.2566310325652),
 .UNSPECIFIED.);
#1476=B_SPLINE_CURVE_WITH_KNOTS('',3,(#19103,#19104,#19105,#19106,#19107,
#19108,#19109,#19110,#19111,#19112),.UNSPECIFIED.,.F.,.F.,(4,1,1,1,1,1,
1,4),(59.6902604182061,60.2166929293287,61.2085635432371,62.2004341571455,
63.1923047710539,64.1841753849622,65.1760459988706,65.9734457253856),
 .UNSPECIFIED.);
#1477=B_SPLINE_CURVE_WITH_KNOTS('',3,(#19113,#19114,#19115,#19116,#19117,
#19118,#19119,#19120,#19121,#19122,#19123),.UNSPECIFIED.,.F.,.F.,(4,1,1,
1,1,1,1,1,4),(59.690260418206,59.9284587949318,60.9211699726728,61.9138811504138,
62.9065923281547,63.8993035058957,64.8920146836367,65.8847258613777,65.9734457253856),
 .UNSPECIFIED.);
#1478=B_SPLINE_CURVE_WITH_KNOTS('',3,(#19128,#19129,#19130,#19131,#19132,
#19133,#19134,#19135,#19136,#19137),.UNSPECIFIED.,.F.,.F.,(4,1,1,1,1,1,
1,4),(53.4070751110265,54.2654692458785,55.2573398597868,56.2492104736952,
57.2410810876036,58.232951701512,59.2248223154203,59.6902604182061),
 .UNSPECIFIED.);
#1479=B_SPLINE_CURVE_WITH_KNOTS('',3,(#19138,#19139,#19140,#19141,#19142,
#19143,#19144,#19145,#19146,#19147),.UNSPECIFIED.,.F.,.F.,(4,1,1,1,1,1,
1,4),(53.4070751110264,53.972191728486,54.9649029062269,55.9576140839679,
56.9503252617089,57.9430364394499,58.9357476171908,59.690260418206),
 .UNSPECIFIED.);
#1480=B_SPLINE_CURVE_WITH_KNOTS('',3,(#19152,#19153,#19154,#19155,#19156,
#19157,#19158,#19159,#19160,#19161,#19162),.UNSPECIFIED.,.F.,.F.,(4,1,1,
1,1,1,1,1,4),(47.1238898038469,47.3223749485198,48.3142455624282,49.3061161763366,
50.2979867902449,51.2898574041533,52.2817280180617,53.2735986319701,53.4070751110265),
 .UNSPECIFIED.);
#1481=B_SPLINE_CURVE_WITH_KNOTS('',3,(#19163,#19164,#19165,#19166,#19167,
#19168,#19169,#19170,#19171,#19172),.UNSPECIFIED.,.F.,.F.,(4,1,1,1,1,1,
1,4),(47.1238898038468,48.0159246620401,49.0086358397811,50.001347017522,
50.994058195263,51.986769373004,52.979480550745,53.4070751110264),
 .UNSPECIFIED.);
#1482=B_SPLINE_CURVE_WITH_KNOTS('',3,(#19177,#19178,#19179,#19180,#19181,
#19182,#19183,#19184,#19185,#19186),.UNSPECIFIED.,.F.,.F.,(4,1,1,1,1,1,
1,4),(40.8407044966673,41.3711512650695,42.3630218789779,43.3548924928863,
44.3467631067947,45.3386337207031,46.3305043346114,47.1238898038469),
 .UNSPECIFIED.);
#1483=B_SPLINE_CURVE_WITH_KNOTS('',3,(#19187,#19188,#19189,#19190,#19191,
#19192,#19193,#19194,#19195,#19196,#19197),.UNSPECIFIED.,.F.,.F.,(4,1,1,
1,1,1,1,1,4),(40.8407044966672,41.0669464178533,42.0596575955942,43.0523687733352,
44.0450799510762,45.0377911288172,46.0305023065581,47.0232134842991,47.1238898038468),
 .UNSPECIFIED.);
#1484=B_SPLINE_CURVE_WITH_KNOTS('',3,(#19202,#19203,#19204,#19205,#19206,
#19207,#19208,#19209,#19210,#19211),.UNSPECIFIED.,.F.,.F.,(4,1,1,1,1,1,
1,4),(34.5575191894877,35.4199275816193,36.4117981955277,37.403668809436,
38.3955394233444,39.3874100372528,40.3792806511612,40.8407044966673),
 .UNSPECIFIED.);
#1485=B_SPLINE_CURVE_WITH_KNOTS('',3,(#19212,#19213,#19214,#19215,#19216,
#19217,#19218,#19219,#19220,#19221),.UNSPECIFIED.,.F.,.F.,(4,1,1,1,1,1,
1,4),(34.5575191894876,35.1106793514074,36.1033905291484,37.0961017068893,
38.0888128846303,39.0815240623713,40.0742352401123,40.8407044966672),
 .UNSPECIFIED.);
#1486=B_SPLINE_CURVE_WITH_KNOTS('',3,(#19226,#19227,#19228,#19229,#19230,
#19231,#19232,#19233,#19234,#19235,#19236),.UNSPECIFIED.,.F.,.F.,(4,1,1,
1,1,1,1,1,4),(28.2743338823081,28.4768332842606,29.468703898169,30.4605745120774,
31.4524451259858,32.4443157398941,33.4361863538025,34.4280569677109,34.5575191894877),
 .UNSPECIFIED.);
#1487=B_SPLINE_CURVE_WITH_KNOTS('',3,(#19237,#19238,#19239,#19240,#19241,
#19242,#19243,#19244,#19245,#19246),.UNSPECIFIED.,.F.,.F.,(4,1,1,1,1,1,
1,4),(28.2743338823081,29.1544122849615,30.1471234627025,31.1398346404435,
32.1325458181845,33.1252569959254,34.1179681736664,34.5575191894876),
 .UNSPECIFIED.);
#1488=B_SPLINE_CURVE_WITH_KNOTS('',3,(#19251,#19252,#19253,#19254,#19255,
#19256,#19257,#19258,#19259,#19260),.UNSPECIFIED.,.F.,.F.,(4,1,1,1,1,1,
1,4),(21.9911485751285,22.5256096008104,23.5174802147187,24.5093508286271,
25.5012214425355,26.4930920564439,27.4849626703523,28.2743338823081),
 .UNSPECIFIED.);
#1489=B_SPLINE_CURVE_WITH_KNOTS('',3,(#19261,#19262,#19263,#19264,#19265,
#19266,#19267,#19268,#19269,#19270,#19271),.UNSPECIFIED.,.F.,.F.,(4,1,1,
1,1,1,1,1,4),(21.9911485751285,22.2054340407747,23.1981452185157,24.1908563962566,
25.1835675739976,26.1762787517386,27.1689899294796,28.1617011072206,28.2743338823081),
 .UNSPECIFIED.);
#1490=B_SPLINE_CURVE_WITH_KNOTS('',3,(#19276,#19277,#19278,#19279,#19280,
#19281,#19282,#19283,#19284,#19285),.UNSPECIFIED.,.F.,.F.,(4,1,1,1,1,1,
1,4),(15.7079632679489,16.5743859173601,17.5662565312685,18.5581271451769,
19.5499977590852,20.5418683729936,21.533738986902,21.9911485751285),
 .UNSPECIFIED.);
#1491=B_SPLINE_CURVE_WITH_KNOTS('',3,(#19286,#19287,#19288,#19289,#19290,
#19291,#19292,#19293,#19294,#19295),.UNSPECIFIED.,.F.,.F.,(4,1,1,1,1,1,
1,4),(15.7079632679489,16.2491669743288,17.2418781520698,18.2345893298108,
19.2273005075518,20.2200116852927,21.2127228630337,21.9911485751285),
 .UNSPECIFIED.);
#1492=B_SPLINE_CURVE_WITH_KNOTS('',3,(#19298,#19299,#19300,#19301,#19302,
#19303,#19304,#19305,#19306,#19307,#19308,#19309,#19310,#19311,#19312,#19313,
#19314,#19315,#19316,#19317,#19318,#19319,#19320,#19321,#19322,#19323,#19324,
#19325,#19326,#19327,#19328,#19329,#19330,#19331,#19332,#19333,#19334,#19335,
#19336,#19337,#19338,#19339,#19340,#19341,#19342,#19343,#19344,#19345,#19346,
#19347,#19348,#19349,#19350,#19351,#19352,#19353,#19354,#19355,#19356,#19357,
#19358,#19359,#19360,#19361,#19362,#19363,#19364,#19365,#19366,#19367,#19368,
#19369,#19370,#19371,#19372,#19373,#19374,#19375,#19376,#19377,#19378,#19379,
#19380,#19381,#19382,#19383,#19384,#19385,#19386,#19387,#19388,#19389,#19390,
#19391,#19392,#19393,#19394,#19395,#19396,#19397,#19398,#19399,#19400,#19401,
#19402,#19403,#19404,#19405,#19406,#19407,#19408,#19409,#19410,#19411,#19412,
#19413,#19414,#19415,#19416,#19417,#19418,#19419,#19420,#19421,#19422,#19423,
#19424,#19425,#19426,#19427,#19428,#19429,#19430,#19431,#19432,#19433,#19434,
#19435,#19436,#19437,#19438,#19439,#19440,#19441,#19442,#19443,#19444,#19445,
#19446,#19447,#19448,#19449,#19450,#19451,#19452,#19453,#19454,#19455,#19456,
#19457,#19458,#19459,#19460,#19461,#19462,#19463,#19464,#19465,#19466,#19467,
#19468,#19469,#19470,#19471,#19472,#19473,#19474,#19475,#19476,#19477,#19478,
#19479,#19480,#19481,#19482,#19483,#19484,#19485,#19486,#19487,#19488,#19489,
#19490,#19491,#19492,#19493,#19494,#19495,#19496,#19497,#19498,#19499,#19500,
#19501,#19502,#19503,#19504,#19505,#19506,#19507,#19508,#19509,#19510,#19511,
#19512,#19513,#19514,#19515,#19516,#19517),.UNSPECIFIED.,.F.,.F.,(4,3,3,
3,3,3,3,3,3,3,3,3,3,3,3,3,3,3,3,3,3,3,3,3,3,3,3,3,3,3,3,3,3,3,3,3,3,3,3,
3,3,3,3,3,3,3,3,3,3,3,3,3,3,3,3,3,3,3,3,3,3,3,3,3,3,3,3,3,3,3,3,3,3,4),
(-1.5115530493723,-1.48679433039677,-1.46137997144481,-1.44936627203976,
-1.44203978844916,-1.43723948275662,-1.41130482704604,-1.3851425648951,
-1.36907979899106,-1.36528335260342,-1.33883417182409,-1.31251413265359,
-1.29083745680875,-1.27999911888633,-1.27252822943752,-1.26916078096391,
-1.2438409010096,-1.21777622976252,-1.19264806966918,-1.18165449962834,
-1.17500808302858,-1.17140113753098,-1.14461626345551,-1.11752388424601,
-1.09233065043846,-1.08197947093734,-1.07663416157974,-1.07221334700158,
-1.04448214800868,-1.01675094901579,-0.989899829038698,-0.980534050538336,
-0.975142748268706,-0.971473262423844,-0.944367339171939,-0.916829945945447,
-0.889160172398661,-0.878253059899969,-0.87283587922991,-0.869128423226553,
-0.840502786522066,-0.812629809126308,-0.785184824902654,-0.776260550181423,
-0.769615191493828,-0.76539079696697,-0.754625876408607,-0.727617533495154,
-0.699889836956671,-0.672733437279935,-0.663027286995113,-0.658922109894078,
-0.630659562625353,-0.602060824740566,-0.57220527844112,-0.560770556686858,
-0.556383058918736,-0.552005977862112,-0.523133364911618,-0.494697204184849,
-0.482638639542781,-0.454174910522506,-0.448377858002803,-0.443883394073885,
-0.415482165359649,-0.386508614853008,-0.357316612716015,-0.340170191390177,
-0.335377465438287,-0.305918315871394,-0.27645436453335,-0.247645675491356,
-0.226999958751525,-0.219677966288016),.UNSPECIFIED.);
#1493=B_SPLINE_CURVE_WITH_KNOTS('',3,(#19519,#19520,#19521,#19522,#19523,
#19524,#19525,#19526,#19527,#19528,#19529,#19530,#19531,#19532,#19533,#19534,
#19535,#19536,#19537,#19538,#19539,#19540,#19541,#19542,#19543,#19544,#19545,
#19546,#19547,#19548,#19549,#19550,#19551,#19552,#19553,#19554,#19555,#19556,
#19557,#19558,#19559,#19560,#19561,#19562,#19563,#19564,#19565,#19566,#19567,
#19568,#19569,#19570,#19571,#19572,#19573,#19574,#19575,#19576,#19577,#19578,
#19579,#19580,#19581,#19582),.UNSPECIFIED.,.F.,.F.,(4,3,3,3,3,3,3,3,3,3,
3,3,3,3,3,3,3,3,3,3,3,4),(-0.410648750433038,-0.381296088292737,-0.350882391849445,
-0.328072119516976,-0.310964415267624,-0.305842993500878,-0.301661871504881,
-0.274116258800685,-0.259641302519569,-0.231392457082299,-0.202468399947011,
-0.198019208917011,-0.170841895434807,-0.143725312403613,-0.117042212888725,
-0.102411936277635,-0.097195049751494,-0.0935363835720784,-0.0677899334604712,
-0.0424347820407558,-0.0178142542830924,0.),.UNSPECIFIED.);
#1494=B_SPLINE_CURVE_WITH_KNOTS('',3,(#19585,#19586,#19587,#19588,#19589,
#19590,#19591,#19592,#19593,#19594,#19595,#19596,#19597,#19598,#19599,#19600,
#19601,#19602,#19603,#19604,#19605,#19606,#19607,#19608,#19609,#19610,#19611,
#19612,#19613,#19614,#19615),.UNSPECIFIED.,.F.,.F.,(4,3,3,3,3,3,3,3,3,3,
4),(-0.219677966288016,-0.201006229477425,-0.172158028090248,-0.142713390739092,
-0.124874216896705,-0.114789665948937,-0.110082687886506,-0.0803547102951982,
-0.0502957032480209,-0.0203907630638487,0.),.UNSPECIFIED.);
#1495=B_SPLINE_CURVE_WITH_KNOTS('',3,(#20028,#20029,#20030,#20031,#20032,
#20033,#20034,#20035),.UNSPECIFIED.,.F.,.F.,(4,1,1,1,1,4),(11.6150328478182,
12.6069034617266,13.598774075635,14.5906446895433,15.5825153034517,15.7079632679489),
 .UNSPECIFIED.);
#1496=B_SPLINE_CURVE_WITH_KNOTS('',3,(#20036,#20037,#20038,#20039,#20040,
#20041,#20042,#20043,#20044,#20045,#20046,#20047,#20048,#20049,#20050,#20051,
#20052,#20053,#20054,#20055,#20056,#20057,#20058,#20059,#20060,#20061,#20062,
#20063,#20064,#20065,#20066,#20067,#20068,#20069,#20070,#20071,#20072,#20073,
#20074,#20075,#20076,#20077,#20078,#20079,#20080,#20081,#20082,#20083,#20084,
#20085,#20086,#20087,#20088,#20089,#20090,#20091,#20092,#20093,#20094,#20095,
#20096,#20097,#20098,#20099,#20100,#20101,#20102,#20103,#20104,#20105,#20106,
#20107,#20108,#20109,#20110,#20111,#20112,#20113,#20114,#20115,#20116,#20117,
#20118,#20119,#20120,#20121,#20122,#20123),.UNSPECIFIED.,.F.,.F.,(4,3,3,
3,3,3,3,3,3,3,3,3,3,3,3,3,3,3,3,3,3,3,3,3,3,3,3,3,3,4),(-0.552745378375041,
-0.527830263536694,-0.498419933292456,-0.482944277728704,-0.477004703287069,
-0.471889411648522,-0.442842142020847,-0.418838054802294,-0.408336266644177,
-0.40199148464016,-0.397446251891128,-0.369139848009071,-0.341087780585202,
-0.313931322984348,-0.298150853306366,-0.293754274173184,-0.266922432864957,
-0.250809444272419,-0.223433348051691,-0.19550417954523,-0.19139998392206,
-0.164790719651446,-0.138164593558308,-0.11192170155777,-0.0979314888630491,
-0.0936568444848153,-0.0680692021908508,-0.0428602319276656,-0.0184469101431373,
0.),.UNSPECIFIED.);
#1497=B_SPLINE_CURVE_WITH_KNOTS('',3,(#20124,#20125,#20126,#20127,#20128,
#20129,#20130,#20131,#20132,#20133,#20134,#20135,#20136,#20137,#20138,#20139,
#20140,#20141,#20142),.UNSPECIFIED.,.F.,.F.,(4,3,3,3,3,3,4),(-96.6808425304193,
-96.2114495491126,-95.2195789352043,-94.2277083212959,-93.2358377073875,
-92.2439670934791,-92.0575247206449),.UNSPECIFIED.);
#1498=B_SPLINE_CURVE_WITH_KNOTS('',3,(#20145,#20146,#20147,#20148,#20149,
#20150,#20151,#20152,#20153),.UNSPECIFIED.,.F.,.F.,(4,1,1,1,1,1,4),(10.3761157273101,
11.2856110856239,12.2783222633649,13.2710334411059,14.2637446188469,15.2564557965878,
15.7079632679489),.UNSPECIFIED.);
#1499=B_SPLINE_CURVE_WITH_KNOTS('',3,(#20571,#20572,#20573,#20574,#20575,
#20576,#20577,#20578,#20579,#20580,#20581,#20582,#20583,#20584,#20585,#20586,
#20587,#20588,#20589,#20590,#20591,#20592),.UNSPECIFIED.,.F.,.F.,(4,3,3,
3,3,3,3,4),(89.0818947088825,89.3440059966879,90.3367171744289,91.3294283521699,
92.3221395299109,93.3148507076518,94.3075618853928,94.6122043555102),
 .UNSPECIFIED.);
#1500=B_SPLINE_CURVE_WITH_KNOTS('',3,(#20593,#20594,#20595,#20596,#20597,
#20598,#20599,#20600,#20601,#20602,#20603,#20604,#20605,#20606,#20607,#20608,
#20609,#20610,#20611,#20612,#20613,#20614,#20615,#20616,#20617,#20618,#20619,
#20620,#20621,#20622,#20623,#20624,#20625,#20626,#20627,#20628,#20629,#20630,
#20631,#20632,#20633,#20634,#20635,#20636,#20637,#20638,#20639,#20640,#20641,
#20642,#20643,#20644,#20645,#20646,#20647,#20648,#20649,#20650,#20651,#20652,
#20653,#20654,#20655,#20656,#20657,#20658,#20659,#20660,#20661,#20662,#20663,
#20664,#20665,#20666,#20667,#20668,#20669,#20670,#20671,#20672,#20673,#20674,
#20675,#20676,#20677,#20678,#20679,#20680),.UNSPECIFIED.,.F.,.F.,(4,3,3,
3,3,3,3,3,3,3,3,3,3,3,3,3,3,3,3,3,3,3,3,3,3,3,3,3,3,4),(-0.555272788399392,
-0.535208229286056,-0.51046000550438,-0.495927663091087,-0.490771565699598,
-0.464551573131573,-0.44160907963455,-0.431518091480653,-0.425427657470475,
-0.420791193383041,-0.394188077983384,-0.365893964776387,-0.344673379871139,
-0.328757941192203,-0.324434111993057,-0.296521822210165,-0.281011625155395,
-0.254049889550291,-0.226554106924644,-0.220947145848259,-0.216688100237889,
-0.188737539857684,-0.160250957640402,-0.131525362881473,-0.114279480489655,
-0.109581292141837,-0.0801117384511396,-0.0505679692714886,-0.0215915474943119,
0.),.UNSPECIFIED.);
#1501=B_SPLINE_CURVE_WITH_KNOTS('',3,(#20749,#20750,#20751,#20752),
 .UNSPECIFIED.,.F.,.F.,(4,4),(32.725489676875,33.4328714289264),
 .UNSPECIFIED.);
#1502=B_SPLINE_CURVE_WITH_KNOTS('',3,(#20755,#20756,#20757,#20758,#20759,
#20760,#20761,#20762,#20763,#20764),.UNSPECIFIED.,.F.,.F.,(4,3,3,4),(-31.4159265358979,
-30.4829121851976,-29.499592437288,-28.9817156343595),.UNSPECIFIED.);
#1503=B_SPLINE_CURVE_WITH_KNOTS('',3,(#20769,#20770,#20771,#20772,#20773,
#20774,#20775,#20776,#20777,#20778,#20779,#20780,#20781,#20782,#20783,#20784,
#20785,#20786,#20787,#20788,#20789,#20790,#20791,#20792,#20793),
 .UNSPECIFIED.,.F.,.F.,(4,3,3,3,3,3,3,3,4),(26.4423043696954,26.5496331935592,
27.5329529414688,28.5162726893784,29.499592437288,30.4829121851976,31.4662319331072,
32.4495516810168,32.725489676875),.UNSPECIFIED.);
#1504=B_SPLINE_CURVE_WITH_KNOTS('',3,(#20794,#20795,#20796,#20797,#20798,
#20799,#20800,#20801,#20802,#20803,#20804,#20805,#20806,#20807,#20808,#20809,
#20810,#20811,#20812,#20813,#20814,#20815),.UNSPECIFIED.,.F.,.F.,(4,3,3,
3,3,3,3,4),(-28.9817156343595,-28.5162726893784,-27.5329529414688,-26.5496331935592,
-25.5663134456496,-24.58299369774,-23.5996739498304,-22.6985303271799),
 .UNSPECIFIED.);
#1505=B_SPLINE_CURVE_WITH_KNOTS('',3,(#20820,#20821,#20822,#20823,#20824,
#20825,#20826,#20827,#20828,#20829,#20830,#20831,#20832,#20833,#20834,#20835,
#20836,#20837,#20838,#20839,#20840,#20841),.UNSPECIFIED.,.F.,.F.,(4,3,3,
3,3,3,3,4),(20.1591190625159,20.6497147061016,21.6330344540112,22.6163542019208,
23.5996739498304,24.58299369774,25.5663134456496,26.4423043696954),
 .UNSPECIFIED.);
#1506=B_SPLINE_CURVE_WITH_KNOTS('',3,(#20842,#20843,#20844,#20845,#20846,
#20847,#20848,#20849,#20850,#20851,#20852,#20853,#20854,#20855,#20856,#20857,
#20858,#20859,#20860,#20861,#20862,#20863,#20864,#20865,#20866),
 .UNSPECIFIED.,.F.,.F.,(4,3,3,3,3,3,3,3,4),(-22.6985303271799,-22.6163542019208,
-21.6330344540112,-20.6497147061016,-19.666394958192,-18.6830752102824,
-17.6997554623728,-16.7164357144632,-16.4153450200003),.UNSPECIFIED.);
#1507=B_SPLINE_CURVE_WITH_KNOTS('',3,(#20871,#20872,#20873,#20874,#20875,
#20876,#20877,#20878,#20879,#20880,#20881,#20882,#20883,#20884,#20885,#20886,
#20887,#20888,#20889,#20890,#20891,#20892),.UNSPECIFIED.,.F.,.F.,(4,3,3,
3,3,3,3,4),(13.8759337553363,14.749796218644,15.7331159665536,16.7164357144632,
17.6997554623728,18.6830752102824,19.666394958192,20.1591190625159),
 .UNSPECIFIED.);
#1508=B_SPLINE_CURVE_WITH_KNOTS('',3,(#20893,#20894,#20895,#20896,#20897,
#20898,#20899,#20900,#20901,#20902,#20903,#20904,#20905,#20906,#20907,#20908,
#20909,#20910,#20911,#20912,#20913,#20914),.UNSPECIFIED.,.F.,.F.,(4,3,3,
3,3,3,3,4),(-16.4153450200003,-15.7331159665536,-14.749796218644,-13.7664764707344,
-12.7831567228248,-11.7998369749152,-10.8165172270056,-10.1321597128207),
 .UNSPECIFIED.);
#1509=B_SPLINE_CURVE_WITH_KNOTS('',3,(#20920,#20921,#20922,#20923,#20924,
#20925,#20926,#20927,#20928,#20929,#20930,#20931,#20932),.UNSPECIFIED.,
 .F.,.F.,(4,3,3,3,4),(-3.84897440564114,-2.9499592437288,-1.9666394958192,
-0.983319747909601,0.),.UNSPECIFIED.);
#1510=B_SPLINE_CURVE_WITH_KNOTS('',3,(#20935,#20936,#20937,#20938,#20939,
#20940,#20941,#20942,#20943,#20944,#20945,#20946,#20947,#20948,#20949,#20950,
#20951,#20952,#20953),.UNSPECIFIED.,.F.,.F.,(4,3,3,3,3,3,4),(2.01694489302844,
2.9499592437288,3.9332789916384,4.916598739548,5.8999184874576,6.8832382353672,
7.59274844815668),.UNSPECIFIED.);
#1511=B_SPLINE_CURVE_WITH_KNOTS('',3,(#20959,#20960,#20961,#20962,#20963,
#20964,#20965,#20966),.UNSPECIFIED.,.F.,.F.,(4,1,1,1,1,4),(40.8407044966673,
41.3585812995958,42.3419010475054,43.325220795415,44.3085405433246,45.2918602912342),
 .UNSPECIFIED.);
#1512=B_SPLINE_CURVE_WITH_KNOTS('',3,(#20969,#20970,#20971,#20972,#20973,
#20974,#20975,#20976,#20977),.UNSPECIFIED.,.F.,.F.,(4,1,1,1,1,1,4),(40.8407044966673,
40.948033320531,41.9313530684406,42.9146728163502,43.8979925642598,44.8813123121694,
45.8143266628698),.UNSPECIFIED.);
#1513=B_SPLINE_CURVE_WITH_KNOTS('',3,(#20982,#20983,#20984,#20985,#20986,
#20987,#20988,#20989,#20990,#20991),.UNSPECIFIED.,.F.,.F.,(4,1,1,1,1,1,
1,4),(34.5575191894877,35.4586628121382,36.4419825600478,37.4253023079574,
38.408622055867,39.3919418037766,40.3752615516862,40.8407044966673),
 .UNSPECIFIED.);
#1514=B_SPLINE_CURVE_WITH_KNOTS('',3,(#20992,#20993,#20994,#20995,#20996,
#20997,#20998,#20999,#21000,#21001),.UNSPECIFIED.,.F.,.F.,(4,1,1,1,1,1,
1,4),(34.5575191894877,35.0481148330734,36.031434580983,37.0147543288926,
37.9980740768022,38.9813938247118,39.9647135726214,40.8407044966673),
 .UNSPECIFIED.);
#1515=B_SPLINE_CURVE_WITH_KNOTS('',3,(#21006,#21007,#21008,#21009,#21010,
#21011,#21012,#21013,#21014,#21015,#21016),.UNSPECIFIED.,.F.,.F.,(4,1,1,
1,1,1,1,1,4),(28.2743338823081,28.575424576771,29.5587443246806,30.5420640725902,
31.5253838204998,32.5087035684094,33.492023316319,34.4753430642286,34.5575191894877),
 .UNSPECIFIED.);
#1516=B_SPLINE_CURVE_WITH_KNOTS('',3,(#21017,#21018,#21019,#21020,#21021,
#21022,#21023,#21024,#21025,#21026),.UNSPECIFIED.,.F.,.F.,(4,1,1,1,1,1,
1,4),(28.2743338823081,29.1481963456159,30.1315160935254,31.114835841435,
32.0981555893446,33.0814753372542,34.0647950851639,34.5575191894877),
 .UNSPECIFIED.);
#1517=B_SPLINE_CURVE_WITH_KNOTS('',3,(#21031,#21032,#21033,#21034,#21035,
#21036,#21037,#21038,#21039,#21040),.UNSPECIFIED.,.F.,.F.,(4,1,1,1,1,1,
1,4),(21.9911485751285,22.6755060893134,23.658825837223,24.6421455851326,
25.6254653330422,26.6087850809518,27.5921048288614,28.2743338823081),
 .UNSPECIFIED.);
#1518=B_SPLINE_CURVE_WITH_KNOTS('',3,(#21041,#21042,#21043,#21044,#21045,
#21046,#21047,#21048,#21049,#21050,#21051),.UNSPECIFIED.,.F.,.F.,(4,1,1,
1,1,1,1,1,4),(21.9911485751285,22.2649581102487,23.2482778581583,24.2315976060679,
25.2149173539775,26.1982371018871,27.1815568497966,28.1648765977063,28.2743338823081),
 .UNSPECIFIED.);
#1519=B_SPLINE_CURVE_WITH_KNOTS('',3,(#21057,#21058,#21059,#21060,#21061),
 .UNSPECIFIED.,.F.,.F.,(4,1,4),(14.3984001269719,15.3817198748815,15.7079632679489),
 .UNSPECIFIED.);
#1520=B_SPLINE_CURVE_WITH_KNOTS('',3,(#21064,#21065,#21066,#21067,#21068),
 .UNSPECIFIED.,.F.,.F.,(4,1,4),(13.8759337553363,14.8089481060366,15.7079632679489),
 .UNSPECIFIED.);
#1521=B_SPLINE_CURVE_WITH_KNOTS('',3,(#21070,#21071,#21072,#21073,#21074,
#21075,#21076,#21077,#21078,#21079,#21080),.UNSPECIFIED.,.F.,.F.,(4,1,1,
1,1,1,1,1,4),(15.7079632679489,15.7922678539462,16.7755876018558,17.7589073497654,
18.742227097675,19.7255468455846,20.7088665934942,21.6921863414038,21.9911485751285),
 .UNSPECIFIED.);
#1522=B_SPLINE_CURVE_WITH_KNOTS('',3,(#21081,#21082,#21083,#21084,#21085,
#21086,#21087,#21088,#21089,#21090),.UNSPECIFIED.,.F.,.F.,(4,1,1,1,1,1,
1,4),(15.7079632679489,16.3650396227911,17.3483593707007,18.3316791186103,
19.3149988665199,20.2983186144295,21.2816383623391,21.9911485751285),
 .UNSPECIFIED.);
#1523=B_SPLINE_CURVE_WITH_KNOTS('',3,(#21239,#21240,#21241,#21242,#21243,
#21244,#21245,#21246,#21247,#21248,#21249,#21250,#21251,#21252,#21253,#21254,
#21255,#21256,#21257,#21258,#21259,#21260,#21261,#21262,#21263,#21264,#21265,
#21266,#21267,#21268,#21269,#21270,#21271,#21272,#21273,#21274,#21275,#21276,
#21277,#21278,#21279,#21280,#21281,#21282,#21283,#21284,#21285,#21286,#21287,
#21288,#21289,#21290,#21291,#21292,#21293,#21294,#21295,#21296,#21297,#21298,
#21299,#21300,#21301,#21302,#21303,#21304,#21305,#21306,#21307,#21308,#21309,
#21310,#21311,#21312,#21313,#21314,#21315,#21316,#21317,#21318,#21319,#21320,
#21321,#21322,#21323,#21324,#21325,#21326),.UNSPECIFIED.,.F.,.F.,(4,3,3,
3,3,3,3,3,3,3,3,3,3,3,3,3,3,3,3,3,3,3,3,3,3,3,3,3,3,4),(0.,0.0297382846428454,
0.0601255889259488,0.0890332382811597,0.114327431466969,0.120650702355347,
0.150403564921709,0.179988720829457,0.207838236564002,0.229395399392172,
0.23393415783729,0.262660470802463,0.291386783767636,0.320322059900051,
0.335078154046361,0.340193241308639,0.344573678198122,0.372678327643481,
0.400795960862634,0.428486852199556,0.439053852931727,0.445278633015735,
0.450309834423539,0.477267903159324,0.497055818929743,0.50468887016549,
0.511949053885254,0.537905662994819,0.556419566241001,0.569248610399422),
 .UNSPECIFIED.);
#1524=B_SPLINE_CURVE_WITH_KNOTS('',3,(#21327,#21328,#21329,#21330,#21331,
#21332,#21333,#21334,#21335,#21336,#21337,#21338,#21339,#21340,#21341,#21342,
#21343,#21344,#21345,#21346,#21347,#21348,#21349,#21350,#21351,#21352,#21353,
#21354,#21355,#21356,#21357,#21358,#21359,#21360,#21361,#21362,#21363,#21364,
#21365,#21366,#21367,#21368,#21369,#21370,#21371,#21372,#21373,#21374,#21375,
#21376,#21377,#21378,#21379,#21380,#21381,#21382,#21383,#21384,#21385,#21386,
#21387,#21388,#21389,#21390,#21391,#21392,#21393,#21394,#21395,#21396,#21397,
#21398,#21399,#21400,#21401,#21402,#21403,#21404,#21405,#21406,#21407,#21408,
#21409,#21410,#21411,#21412,#21413,#21414,#21415,#21416,#21417,#21418,#21419,
#21420),.UNSPECIFIED.,.F.,.F.,(4,3,3,3,3,3,3,3,3,3,3,3,3,3,3,3,3,3,3,3,
3,3,3,3,3,3,3,3,3,3,3,4),(0.,0.0253795104813928,0.0514287956022284,0.0778538073776754,
0.0899945430700518,0.0969018068642677,0.102642146791298,0.129947872947979,
0.157699027910297,0.183981493384174,0.195665040532001,0.201809460807294,
0.206412496951858,0.235040986639171,0.262828889805804,0.290686253909393,
0.306981212992593,0.31132393091396,0.315703998135388,0.34516669827354,0.374337762706802,
0.403793893800065,0.41497713906407,0.422789593408606,0.427299404513114,
0.458325953194986,0.48159586470639,0.493906250475823,0.500072154367986,
0.530578895950629,0.551405599240602,0.566847306048089),.UNSPECIFIED.);
#1525=B_SPLINE_CURVE_WITH_KNOTS('',3,(#21421,#21422,#21423,#21424,#21425,
#21426,#21427,#21428,#21429,#21430,#21431,#21432,#21433,#21434,#21435,#21436,
#21437,#21438,#21439,#21440,#21441,#21442,#21443,#21444,#21445),
 .UNSPECIFIED.,.F.,.F.,(4,3,3,3,3,3,3,3,4),(-10.1321597128207,-9.833197479096,
-8.8498777311864,-7.8665579832768,-6.8832382353672,-5.8999184874576,-4.916598739548,
-3.9332789916384,-3.84897440564114),.UNSPECIFIED.);
#1526=B_SPLINE_CURVE_WITH_KNOTS('',3,(#21594,#21595,#21596,#21597,#21598,
#21599,#21600,#21601,#21602,#21603,#21604,#21605,#21606,#21607,#21608,#21609,
#21610,#21611,#21612,#21613,#21614,#21615,#21616,#21617,#21618,#21619,#21620,
#21621,#21622,#21623,#21624,#21625,#21626,#21627,#21628,#21629,#21630,#21631,
#21632,#21633,#21634,#21635,#21636,#21637,#21638,#21639,#21640,#21641,#21642,
#21643,#21644,#21645,#21646,#21647,#21648,#21649,#21650,#21651,#21652,#21653,
#21654,#21655,#21656,#21657,#21658,#21659,#21660,#21661,#21662,#21663,#21664,
#21665,#21666,#21667,#21668,#21669,#21670,#21671,#21672,#21673,#21674,#21675,
#21676,#21677,#21678,#21679,#21680,#21681,#21682,#21683,#21684,#21685,#21686,
#21687),.UNSPECIFIED.,.F.,.F.,(4,3,3,3,3,3,3,3,3,3,3,3,3,3,3,3,3,3,3,3,
3,3,3,3,3,3,3,3,3,3,3,4),(0.,0.0253795895352918,0.0514289454719094,0.0778539385136474,
0.0899945864079409,0.0969018005134045,0.102642148135923,0.129947928392544,
0.157699108353734,0.183981553716754,0.195665088727664,0.201809360898104,
0.206412522774552,0.235041003890312,0.262828889805813,0.290686211240011,
0.306981172990049,0.311324022663455,0.315704013189775,0.345166711446132,
0.374337752779982,0.403793879145986,0.414977105191051,0.422789478907973,
0.427299173709167,0.458325780092032,0.481595734879181,0.493906100937864,
0.500072114794957,0.530578856744846,0.551405599240626,0.566847306048098),
 .UNSPECIFIED.);
#1527=B_SPLINE_CURVE_WITH_KNOTS('',3,(#21688,#21689,#21690,#21691,#21692,
#21693,#21694,#21695,#21696,#21697,#21698,#21699,#21700,#21701,#21702,#21703,
#21704,#21705,#21706,#21707,#21708,#21709,#21710,#21711,#21712),
 .UNSPECIFIED.,.F.,.F.,(4,3,3,3,3,3,3,3,4),(7.59274844815668,7.8665579832768,
8.84987773118639,9.833197479096,10.8165172270056,11.7998369749152,12.7831567228248,
13.7664764707344,13.8759337553363),.UNSPECIFIED.);
#1528=B_SPLINE_CURVE_WITH_KNOTS('',3,(#21713,#21714,#21715,#21716,#21717,
#21718,#21719,#21720,#21721,#21722,#21723,#21724,#21725,#21726,#21727,#21728,
#21729,#21730,#21731,#21732,#21733,#21734,#21735,#21736,#21737,#21738,#21739,
#21740,#21741,#21742,#21743,#21744,#21745,#21746,#21747,#21748,#21749,#21750,
#21751,#21752,#21753,#21754,#21755,#21756,#21757,#21758,#21759,#21760,#21761,
#21762,#21763,#21764,#21765,#21766,#21767,#21768,#21769,#21770,#21771,#21772,
#21773,#21774,#21775,#21776,#21777,#21778,#21779,#21780,#21781,#21782,#21783,
#21784,#21785,#21786,#21787,#21788,#21789,#21790,#21791,#21792,#21793,#21794,
#21795,#21796,#21797,#21798,#21799,#21800),.UNSPECIFIED.,.F.,.F.,(4,3,3,
3,3,3,3,3,3,3,3,3,3,3,3,3,3,3,3,3,3,3,3,3,3,3,3,3,3,4),(0.,0.0297383502225738,
0.0601256857797807,0.0890333230282637,0.114327505620686,0.120650688809437,
0.150403550371837,0.179988686667598,0.207838210942609,0.229395337968592,
0.23393415684471,0.262660470306177,0.291386783767645,0.32032206170552,0.335078155738989,
0.340193228824031,0.344573672707814,0.372678323504497,0.400795954000531,
0.428486824889168,0.439053762328703,0.445278745781163,0.450309838937034,
0.477267882086698,0.497055803125278,0.504688833353528,0.511949049757023,
0.537905617573998,0.556419566241016,0.569248610399434),.UNSPECIFIED.);
#1529=LINE('',#8358,#1985);
#1530=LINE('',#8397,#1986);
#1531=LINE('',#8445,#1987);
#1532=LINE('',#8493,#1988);
#1533=LINE('',#8544,#1989);
#1534=LINE('',#8592,#1990);
#1535=LINE('',#8640,#1991);
#1536=LINE('',#8691,#1992);
#1537=LINE('',#8742,#1993);
#1538=LINE('',#8790,#1994);
#1539=LINE('',#8841,#1995);
#1540=LINE('',#8880,#1996);
#1541=LINE('',#8919,#1997);
#1542=LINE('',#8967,#1998);
#1543=LINE('',#9015,#1999);
#1544=LINE('',#9066,#2000);
#1545=LINE('',#9114,#2001);
#1546=LINE('',#9162,#2002);
#1547=LINE('',#9213,#2003);
#1548=LINE('',#9264,#2004);
#1549=LINE('',#9312,#2005);
#1550=LINE('',#9363,#2006);
#1551=LINE('',#9402,#2007);
#1552=LINE('',#9441,#2008);
#1553=LINE('',#9489,#2009);
#1554=LINE('',#9537,#2010);
#1555=LINE('',#9588,#2011);
#1556=LINE('',#9636,#2012);
#1557=LINE('',#9684,#2013);
#1558=LINE('',#9735,#2014);
#1559=LINE('',#9786,#2015);
#1560=LINE('',#9834,#2016);
#1561=LINE('',#9885,#2017);
#1562=LINE('',#9926,#2018);
#1563=LINE('',#9965,#2019);
#1564=LINE('',#10013,#2020);
#1565=LINE('',#10061,#2021);
#1566=LINE('',#10112,#2022);
#1567=LINE('',#10160,#2023);
#1568=LINE('',#10208,#2024);
#1569=LINE('',#10259,#2025);
#1570=LINE('',#10310,#2026);
#1571=LINE('',#10358,#2027);
#1572=LINE('',#10409,#2028);
#1573=LINE('',#10450,#2029);
#1574=LINE('',#10466,#2030);
#1575=LINE('',#10491,#2031);
#1576=LINE('',#10516,#2032);
#1577=LINE('',#10540,#2033);
#1578=LINE('',#10565,#2034);
#1579=LINE('',#10589,#2035);
#1580=LINE('',#10614,#2036);
#1581=LINE('',#10638,#2037);
#1582=LINE('',#10663,#2038);
#1583=LINE('',#10688,#2039);
#1584=LINE('',#10712,#2040);
#1585=LINE('',#10729,#2041);
#1586=LINE('',#10745,#2042);
#1587=LINE('',#10770,#2043);
#1588=LINE('',#10795,#2044);
#1589=LINE('',#10819,#2045);
#1590=LINE('',#10844,#2046);
#1591=LINE('',#10868,#2047);
#1592=LINE('',#10893,#2048);
#1593=LINE('',#10917,#2049);
#1594=LINE('',#10942,#2050);
#1595=LINE('',#10967,#2051);
#1596=LINE('',#10991,#2052);
#1597=LINE('',#11008,#2053);
#1598=LINE('',#11024,#2054);
#1599=LINE('',#11049,#2055);
#1600=LINE('',#11074,#2056);
#1601=LINE('',#11098,#2057);
#1602=LINE('',#11123,#2058);
#1603=LINE('',#11147,#2059);
#1604=LINE('',#11172,#2060);
#1605=LINE('',#11196,#2061);
#1606=LINE('',#11221,#2062);
#1607=LINE('',#11246,#2063);
#1608=LINE('',#11270,#2064);
#1609=LINE('',#11287,#2065);
#1610=LINE('',#11303,#2066);
#1611=LINE('',#11328,#2067);
#1612=LINE('',#11353,#2068);
#1613=LINE('',#11377,#2069);
#1614=LINE('',#11402,#2070);
#1615=LINE('',#11426,#2071);
#1616=LINE('',#11451,#2072);
#1617=LINE('',#11475,#2073);
#1618=LINE('',#11500,#2074);
#1619=LINE('',#11525,#2075);
#1620=LINE('',#11549,#2076);
#1621=LINE('',#11566,#2077);
#1622=LINE('',#11570,#2078);
#1623=LINE('',#11574,#2079);
#1624=LINE('',#11577,#2080);
#1625=LINE('',#11580,#2081);
#1626=LINE('',#11583,#2082);
#1627=LINE('',#11586,#2083);
#1628=LINE('',#11589,#2084);
#1629=LINE('',#11592,#2085);
#1630=LINE('',#11594,#2086);
#1631=LINE('',#11597,#2087);
#1632=LINE('',#11598,#2088);
#1633=LINE('',#11601,#2089);
#1634=LINE('',#11603,#2090);
#1635=LINE('',#11605,#2091);
#1636=LINE('',#11607,#2092);
#1637=LINE('',#11608,#2093);
#1638=LINE('',#11611,#2094);
#1639=LINE('',#11612,#2095);
#1640=LINE('',#11613,#2096);
#1641=LINE('',#11616,#2097);
#1642=LINE('',#11617,#2098);
#1643=LINE('',#11621,#2099);
#1644=LINE('',#11625,#2100);
#1645=LINE('',#11627,#2101);
#1646=LINE('',#11629,#2102);
#1647=LINE('',#11635,#2103);
#1648=LINE('',#11636,#2104);
#1649=LINE('',#11662,#2105);
#1650=LINE('',#11667,#2106);
#1651=LINE('',#11689,#2107);
#1652=LINE('',#11691,#2108);
#1653=LINE('',#11694,#2109);
#1654=LINE('',#11696,#2110);
#1655=LINE('',#11697,#2111);
#1656=LINE('',#11700,#2112);
#1657=LINE('',#11701,#2113);
#1658=LINE('',#11716,#2114);
#1659=LINE('',#11720,#2115);
#1660=LINE('',#12748,#2116);
#1661=LINE('',#12750,#2117);
#1662=LINE('',#12752,#2118);
#1663=LINE('',#12754,#2119);
#1664=LINE('',#12756,#2120);
#1665=LINE('',#12757,#2121);
#1666=LINE('',#12760,#2122);
#1667=LINE('',#12762,#2123);
#1668=LINE('',#12764,#2124);
#1669=LINE('',#12765,#2125);
#1670=LINE('',#12768,#2126);
#1671=LINE('',#12770,#2127);
#1672=LINE('',#12772,#2128);
#1673=LINE('',#12773,#2129);
#1674=LINE('',#12776,#2130);
#1675=LINE('',#12778,#2131);
#1676=LINE('',#12780,#2132);
#1677=LINE('',#12781,#2133);
#1678=LINE('',#15863,#2134);
#1679=LINE('',#15865,#2135);
#1680=LINE('',#15866,#2136);
#1681=LINE('',#15869,#2137);
#1682=LINE('',#15871,#2138);
#1683=LINE('',#15873,#2139);
#1684=LINE('',#15874,#2140);
#1685=LINE('',#15877,#2141);
#1686=LINE('',#15879,#2142);
#1687=LINE('',#15881,#2143);
#1688=LINE('',#15882,#2144);
#1689=LINE('',#15885,#2145);
#1690=LINE('',#15887,#2146);
#1691=LINE('',#15889,#2147);
#1692=LINE('',#15890,#2148);
#1693=LINE('',#15894,#2149);
#1694=LINE('',#15901,#2150);
#1695=LINE('',#15902,#2151);
#1696=LINE('',#15904,#2152);
#1697=LINE('',#15906,#2153);
#1698=LINE('',#15909,#2154);
#1699=LINE('',#15910,#2155);
#1700=LINE('',#15912,#2156);
#1701=LINE('',#15914,#2157);
#1702=LINE('',#15917,#2158);
#1703=LINE('',#15918,#2159);
#1704=LINE('',#15920,#2160);
#1705=LINE('',#15922,#2161);
#1706=LINE('',#15926,#2162);
#1707=LINE('',#15927,#2163);
#1708=LINE('',#15930,#2164);
#1709=LINE('',#15932,#2165);
#1710=LINE('',#15934,#2166);
#1711=LINE('',#15936,#2167);
#1712=LINE('',#15938,#2168);
#1713=LINE('',#15939,#2169);
#1714=LINE('',#15941,#2170);
#1715=LINE('',#15944,#2171);
#1716=LINE('',#15946,#2172);
#1717=LINE('',#15948,#2173);
#1718=LINE('',#15949,#2174);
#1719=LINE('',#15951,#2175);
#1720=LINE('',#15953,#2176);
#1721=LINE('',#15956,#2177);
#1722=LINE('',#15958,#2178);
#1723=LINE('',#16018,#2179);
#1724=LINE('',#16019,#2180);
#1725=LINE('',#16021,#2181);
#1726=LINE('',#16022,#2182);
#1727=LINE('',#16024,#2183);
#1728=LINE('',#16025,#2184);
#1729=LINE('',#16027,#2185);
#1730=LINE('',#16028,#2186);
#1731=LINE('',#16030,#2187);
#1732=LINE('',#16031,#2188);
#1733=LINE('',#16033,#2189);
#1734=LINE('',#16034,#2190);
#1735=LINE('',#16036,#2191);
#1736=LINE('',#16037,#2192);
#1737=LINE('',#16039,#2193);
#1738=LINE('',#16040,#2194);
#1739=LINE('',#16042,#2195);
#1740=LINE('',#16043,#2196);
#1741=LINE('',#16045,#2197);
#1742=LINE('',#16046,#2198);
#1743=LINE('',#16048,#2199);
#1744=LINE('',#16049,#2200);
#1745=LINE('',#16051,#2201);
#1746=LINE('',#16052,#2202);
#1747=LINE('',#16057,#2203);
#1748=LINE('',#16059,#2204);
#1749=LINE('',#16061,#2205);
#1750=LINE('',#16062,#2206);
#1751=LINE('',#16072,#2207);
#1752=LINE('',#16074,#2208);
#1753=LINE('',#16076,#2209);
#1754=LINE('',#16077,#2210);
#1755=LINE('',#16084,#2211);
#1756=LINE('',#16086,#2212);
#1757=LINE('',#16088,#2213);
#1758=LINE('',#16089,#2214);
#1759=LINE('',#16091,#2215);
#1760=LINE('',#16093,#2216);
#1761=LINE('',#16100,#2217);
#1762=LINE('',#16106,#2218);
#1763=LINE('',#16111,#2219);
#1764=LINE('',#16113,#2220);
#1765=LINE('',#16115,#2221);
#1766=LINE('',#16116,#2222);
#1767=LINE('',#16119,#2223);
#1768=LINE('',#16121,#2224);
#1769=LINE('',#16122,#2225);
#1770=LINE('',#16125,#2226);
#1771=LINE('',#16127,#2227);
#1772=LINE('',#16128,#2228);
#1773=LINE('',#16130,#2229);
#1774=LINE('',#16131,#2230);
#1775=LINE('',#16135,#2231);
#1776=LINE('',#16137,#2232);
#1777=LINE('',#16139,#2233);
#1778=LINE('',#16140,#2234);
#1779=LINE('',#16143,#2235);
#1780=LINE('',#16145,#2236);
#1781=LINE('',#16146,#2237);
#1782=LINE('',#16149,#2238);
#1783=LINE('',#16151,#2239);
#1784=LINE('',#16152,#2240);
#1785=LINE('',#16154,#2241);
#1786=LINE('',#16155,#2242);
#1787=LINE('',#16163,#2243);
#1788=LINE('',#16169,#2244);
#1789=LINE('',#16175,#2245);
#1790=LINE('',#16181,#2246);
#1791=LINE('',#16186,#2247);
#1792=LINE('',#16188,#2248);
#1793=LINE('',#16190,#2249);
#1794=LINE('',#16191,#2250);
#1795=LINE('',#16194,#2251);
#1796=LINE('',#16196,#2252);
#1797=LINE('',#16197,#2253);
#1798=LINE('',#16200,#2254);
#1799=LINE('',#16202,#2255);
#1800=LINE('',#16203,#2256);
#1801=LINE('',#16205,#2257);
#1802=LINE('',#16206,#2258);
#1803=LINE('',#16210,#2259);
#1804=LINE('',#16212,#2260);
#1805=LINE('',#16214,#2261);
#1806=LINE('',#16215,#2262);
#1807=LINE('',#16218,#2263);
#1808=LINE('',#16220,#2264);
#1809=LINE('',#16221,#2265);
#1810=LINE('',#16224,#2266);
#1811=LINE('',#16226,#2267);
#1812=LINE('',#16227,#2268);
#1813=LINE('',#16229,#2269);
#1814=LINE('',#16230,#2270);
#1815=LINE('',#16234,#2271);
#1816=LINE('',#16236,#2272);
#1817=LINE('',#16238,#2273);
#1818=LINE('',#16239,#2274);
#1819=LINE('',#16242,#2275);
#1820=LINE('',#16244,#2276);
#1821=LINE('',#16245,#2277);
#1822=LINE('',#16248,#2278);
#1823=LINE('',#16250,#2279);
#1824=LINE('',#16251,#2280);
#1825=LINE('',#16253,#2281);
#1826=LINE('',#16254,#2282);
#1827=LINE('',#16258,#2283);
#1828=LINE('',#16260,#2284);
#1829=LINE('',#16262,#2285);
#1830=LINE('',#16263,#2286);
#1831=LINE('',#16266,#2287);
#1832=LINE('',#16268,#2288);
#1833=LINE('',#16269,#2289);
#1834=LINE('',#16272,#2290);
#1835=LINE('',#16274,#2291);
#1836=LINE('',#16275,#2292);
#1837=LINE('',#16277,#2293);
#1838=LINE('',#16278,#2294);
#1839=LINE('',#16286,#2295);
#1840=LINE('',#16291,#2296);
#1841=LINE('',#16293,#2297);
#1842=LINE('',#16295,#2298);
#1843=LINE('',#16296,#2299);
#1844=LINE('',#16299,#2300);
#1845=LINE('',#16301,#2301);
#1846=LINE('',#16302,#2302);
#1847=LINE('',#16305,#2303);
#1848=LINE('',#16307,#2304);
#1849=LINE('',#16308,#2305);
#1850=LINE('',#16310,#2306);
#1851=LINE('',#16311,#2307);
#1852=LINE('',#16319,#2308);
#1853=LINE('',#16324,#2309);
#1854=LINE('',#16326,#2310);
#1855=LINE('',#16328,#2311);
#1856=LINE('',#16329,#2312);
#1857=LINE('',#16332,#2313);
#1858=LINE('',#16334,#2314);
#1859=LINE('',#16335,#2315);
#1860=LINE('',#16338,#2316);
#1861=LINE('',#16340,#2317);
#1862=LINE('',#16341,#2318);
#1863=LINE('',#16343,#2319);
#1864=LINE('',#16344,#2320);
#1865=LINE('',#16351,#2321);
#1866=LINE('',#16375,#2322);
#1867=LINE('',#16423,#2323);
#1868=LINE('',#16471,#2324);
#1869=LINE('',#16522,#2325);
#1870=LINE('',#16573,#2326);
#1871=LINE('',#16621,#2327);
#1872=LINE('',#16669,#2328);
#1873=LINE('',#16723,#2329);
#1874=LINE('',#16771,#2330);
#1875=LINE('',#16819,#2331);
#1876=LINE('',#16844,#2332);
#1877=LINE('',#16869,#2333);
#1878=LINE('',#16893,#2334);
#1879=LINE('',#16918,#2335);
#1880=LINE('',#16943,#2336);
#1881=LINE('',#16967,#2337);
#1882=LINE('',#16991,#2338);
#1883=LINE('',#17017,#2339);
#1884=LINE('',#17041,#2340);
#1885=LINE('',#17359,#2341);
#1886=LINE('',#18162,#2342);
#1887=LINE('',#18164,#2343);
#1888=LINE('',#18166,#2344);
#1889=LINE('',#18167,#2345);
#1890=LINE('',#18170,#2346);
#1891=LINE('',#18172,#2347);
#1892=LINE('',#18173,#2348);
#1893=LINE('',#18176,#2349);
#1894=LINE('',#18178,#2350);
#1895=LINE('',#18179,#2351);
#1896=LINE('',#18182,#2352);
#1897=LINE('',#18184,#2353);
#1898=LINE('',#18185,#2354);
#1899=LINE('',#18188,#2355);
#1900=LINE('',#18190,#2356);
#1901=LINE('',#18191,#2357);
#1902=LINE('',#18193,#2358);
#1903=LINE('',#18194,#2359);
#1904=LINE('',#18201,#2360);
#1905=LINE('',#18209,#2361);
#1906=LINE('',#18233,#2362);
#1907=LINE('',#18281,#2363);
#1908=LINE('',#18329,#2364);
#1909=LINE('',#18383,#2365);
#1910=LINE('',#18431,#2366);
#1911=LINE('',#18479,#2367);
#1912=LINE('',#18533,#2368);
#1913=LINE('',#18581,#2369);
#1914=LINE('',#18629,#2370);
#1915=LINE('',#18683,#2371);
#1916=LINE('',#18731,#2372);
#1917=LINE('',#18779,#2373);
#1918=LINE('',#18833,#2374);
#1919=LINE('',#18881,#2375);
#1920=LINE('',#18929,#2376);
#1921=LINE('',#18954,#2377);
#1922=LINE('',#18979,#2378);
#1923=LINE('',#19003,#2379);
#1924=LINE('',#19028,#2380);
#1925=LINE('',#19053,#2381);
#1926=LINE('',#19077,#2382);
#1927=LINE('',#19102,#2383);
#1928=LINE('',#19127,#2384);
#1929=LINE('',#19151,#2385);
#1930=LINE('',#19176,#2386);
#1931=LINE('',#19201,#2387);
#1932=LINE('',#19225,#2388);
#1933=LINE('',#19250,#2389);
#1934=LINE('',#19275,#2390);
#1935=LINE('',#19617,#2391);
#1936=LINE('',#20685,#2392);
#1937=LINE('',#20687,#2393);
#1938=LINE('',#20689,#2394);
#1939=LINE('',#20690,#2395);
#1940=LINE('',#20693,#2396);
#1941=LINE('',#20695,#2397);
#1942=LINE('',#20696,#2398);
#1943=LINE('',#20699,#2399);
#1944=LINE('',#20701,#2400);
#1945=LINE('',#20702,#2401);
#1946=LINE('',#20705,#2402);
#1947=LINE('',#20707,#2403);
#1948=LINE('',#20708,#2404);
#1949=LINE('',#20711,#2405);
#1950=LINE('',#20713,#2406);
#1951=LINE('',#20714,#2407);
#1952=LINE('',#20716,#2408);
#1953=LINE('',#20717,#2409);
#1954=LINE('',#20724,#2410);
#1955=LINE('',#20733,#2411);
#1956=LINE('',#20739,#2412);
#1957=LINE('',#20747,#2413);
#1958=LINE('',#20768,#2414);
#1959=LINE('',#20819,#2415);
#1960=LINE('',#20870,#2416);
#1961=LINE('',#20918,#2417);
#1962=LINE('',#20957,#2418);
#1963=LINE('',#20981,#2419);
#1964=LINE('',#21005,#2420);
#1965=LINE('',#21030,#2421);
#1966=LINE('',#21055,#2422);
#1967=LINE('',#21804,#2423);
#1968=LINE('',#21806,#2424);
#1969=LINE('',#21808,#2425);
#1970=LINE('',#21810,#2426);
#1971=LINE('',#21812,#2427);
#1972=LINE('',#21813,#2428);
#1973=LINE('',#21818,#2429);
#1974=LINE('',#21819,#2430);
#1975=LINE('',#21820,#2431);
#1976=LINE('',#21823,#2432);
#1977=LINE('',#21824,#2433);
#1978=LINE('',#21827,#2434);
#1979=LINE('',#21828,#2435);
#1980=LINE('',#21831,#2436);
#1981=LINE('',#21832,#2437);
#1982=LINE('',#21835,#2438);
#1983=LINE('',#21836,#2439);
#1984=LINE('',#21838,#2440);
#1985=VECTOR('',#6973,2.);
#1986=VECTOR('',#6978,2.);
#1987=VECTOR('',#6981,2.);
#1988=VECTOR('',#6984,2.);
#1989=VECTOR('',#6987,2.);
#1990=VECTOR('',#6990,2.);
#1991=VECTOR('',#6993,2.);
#1992=VECTOR('',#6996,2.);
#1993=VECTOR('',#6999,2.);
#1994=VECTOR('',#7002,2.);
#1995=VECTOR('',#7005,2.);
#1996=VECTOR('',#7010,2.);
#1997=VECTOR('',#7015,2.);
#1998=VECTOR('',#7018,2.);
#1999=VECTOR('',#7021,2.);
#2000=VECTOR('',#7024,2.);
#2001=VECTOR('',#7027,2.);
#2002=VECTOR('',#7030,2.);
#2003=VECTOR('',#7033,2.);
#2004=VECTOR('',#7036,2.);
#2005=VECTOR('',#7039,2.);
#2006=VECTOR('',#7042,2.);
#2007=VECTOR('',#7047,2.);
#2008=VECTOR('',#7052,2.);
#2009=VECTOR('',#7055,2.);
#2010=VECTOR('',#7058,2.);
#2011=VECTOR('',#7061,2.);
#2012=VECTOR('',#7064,2.);
#2013=VECTOR('',#7067,2.);
#2014=VECTOR('',#7070,2.);
#2015=VECTOR('',#7073,2.);
#2016=VECTOR('',#7076,2.);
#2017=VECTOR('',#7079,2.);
#2018=VECTOR('',#7086,2.);
#2019=VECTOR('',#7091,2.);
#2020=VECTOR('',#7094,2.);
#2021=VECTOR('',#7097,2.);
#2022=VECTOR('',#7100,2.);
#2023=VECTOR('',#7103,2.);
#2024=VECTOR('',#7106,2.);
#2025=VECTOR('',#7109,2.);
#2026=VECTOR('',#7112,2.);
#2027=VECTOR('',#7115,2.);
#2028=VECTOR('',#7118,2.);
#2029=VECTOR('',#7125,2.05475);
#2030=VECTOR('',#7130,2.05475);
#2031=VECTOR('',#7133,2.05475);
#2032=VECTOR('',#7136,2.05475);
#2033=VECTOR('',#7139,2.05475);
#2034=VECTOR('',#7142,2.05475);
#2035=VECTOR('',#7145,2.05475);
#2036=VECTOR('',#7148,2.05475);
#2037=VECTOR('',#7151,2.05475);
#2038=VECTOR('',#7154,2.05475);
#2039=VECTOR('',#7157,2.05475);
#2040=VECTOR('',#7160,2.05475);
#2041=VECTOR('',#7165,2.05475);
#2042=VECTOR('',#7170,2.05475);
#2043=VECTOR('',#7173,2.05475);
#2044=VECTOR('',#7176,2.05475);
#2045=VECTOR('',#7179,2.05475);
#2046=VECTOR('',#7182,2.05475);
#2047=VECTOR('',#7185,2.05475);
#2048=VECTOR('',#7188,2.05475);
#2049=VECTOR('',#7191,2.05475);
#2050=VECTOR('',#7194,2.05475);
#2051=VECTOR('',#7197,2.05475);
#2052=VECTOR('',#7200,2.05475);
#2053=VECTOR('',#7205,2.05475);
#2054=VECTOR('',#7210,2.05475);
#2055=VECTOR('',#7213,2.05475);
#2056=VECTOR('',#7216,2.05475);
#2057=VECTOR('',#7219,2.05475);
#2058=VECTOR('',#7222,2.05475);
#2059=VECTOR('',#7225,2.05475);
#2060=VECTOR('',#7228,2.05475);
#2061=VECTOR('',#7231,2.05475);
#2062=VECTOR('',#7234,2.05475);
#2063=VECTOR('',#7237,2.05475);
#2064=VECTOR('',#7240,2.05475);
#2065=VECTOR('',#7245,2.05475);
#2066=VECTOR('',#7250,2.05475);
#2067=VECTOR('',#7253,2.05475);
#2068=VECTOR('',#7256,2.05475);
#2069=VECTOR('',#7259,2.05475);
#2070=VECTOR('',#7262,2.05475);
#2071=VECTOR('',#7265,2.05475);
#2072=VECTOR('',#7268,2.05475);
#2073=VECTOR('',#7271,2.05475);
#2074=VECTOR('',#7274,2.05475);
#2075=VECTOR('',#7277,2.05475);
#2076=VECTOR('',#7280,2.05475);
#2077=VECTOR('',#7285,10.);
#2078=VECTOR('',#7288,10.);
#2079=VECTOR('',#7293,10.);
#2080=VECTOR('',#7296,10.);
#2081=VECTOR('',#7299,10.);
#2082=VECTOR('',#7302,10.);
#2083=VECTOR('',#7305,10.);
#2084=VECTOR('',#7308,10.);
#2085=VECTOR('',#7311,10.);
#2086=VECTOR('',#7312,10.);
#2087=VECTOR('',#7317,10.);
#2088=VECTOR('',#7318,10.);
#2089=VECTOR('',#7321,10.);
#2090=VECTOR('',#7322,10.);
#2091=VECTOR('',#7323,10.);
#2092=VECTOR('',#7324,10.);
#2093=VECTOR('',#7325,10.);
#2094=VECTOR('',#7328,10.);
#2095=VECTOR('',#7329,10.);
#2096=VECTOR('',#7330,10.);
#2097=VECTOR('',#7333,10.);
#2098=VECTOR('',#7334,10.);
#2099=VECTOR('',#7337,10.);
#2100=VECTOR('',#7340,10.);
#2101=VECTOR('',#7341,10.);
#2102=VECTOR('',#7342,10.);
#2103=VECTOR('',#7347,10.);
#2104=VECTOR('',#7348,10.);
#2105=VECTOR('',#7353,10.);
#2106=VECTOR('',#7360,10.);
#2107=VECTOR('',#7365,10.);
#2108=VECTOR('',#7368,10.);
#2109=VECTOR('',#7371,10.);
#2110=VECTOR('',#7372,10.);
#2111=VECTOR('',#7373,10.);
#2112=VECTOR('',#7376,10.);
#2113=VECTOR('',#7377,10.);
#2114=VECTOR('',#7396,3.5);
#2115=VECTOR('',#7401,3.5);
#2116=VECTOR('',#7408,10.);
#2117=VECTOR('',#7409,10.);
#2118=VECTOR('',#7410,10.);
#2119=VECTOR('',#7411,10.);
#2120=VECTOR('',#7412,10.);
#2121=VECTOR('',#7413,10.);
#2122=VECTOR('',#7414,10.);
#2123=VECTOR('',#7415,10.);
#2124=VECTOR('',#7416,10.);
#2125=VECTOR('',#7417,10.);
#2126=VECTOR('',#7418,10.);
#2127=VECTOR('',#7419,10.);
#2128=VECTOR('',#7420,10.);
#2129=VECTOR('',#7421,10.);
#2130=VECTOR('',#7422,10.);
#2131=VECTOR('',#7423,10.);
#2132=VECTOR('',#7424,10.);
#2133=VECTOR('',#7425,10.);
#2134=VECTOR('',#7434,10.);
#2135=VECTOR('',#7435,10.);
#2136=VECTOR('',#7436,10.);
#2137=VECTOR('',#7437,10.);
#2138=VECTOR('',#7438,10.);
#2139=VECTOR('',#7439,10.);
#2140=VECTOR('',#7440,10.);
#2141=VECTOR('',#7441,10.);
#2142=VECTOR('',#7442,10.);
#2143=VECTOR('',#7443,10.);
#2144=VECTOR('',#7444,10.);
#2145=VECTOR('',#7445,10.);
#2146=VECTOR('',#7446,10.);
#2147=VECTOR('',#7447,10.);
#2148=VECTOR('',#7448,10.);
#2149=VECTOR('',#7455,10.);
#2150=VECTOR('',#7468,10.);
#2151=VECTOR('',#7469,10.);
#2152=VECTOR('',#7472,10.);
#2153=VECTOR('',#7475,10.);
#2154=VECTOR('',#7480,10.);
#2155=VECTOR('',#7481,10.);
#2156=VECTOR('',#7484,10.);
#2157=VECTOR('',#7487,10.);
#2158=VECTOR('',#7492,10.);
#2159=VECTOR('',#7493,10.);
#2160=VECTOR('',#7496,10.);
#2161=VECTOR('',#7499,10.);
#2162=VECTOR('',#7504,10.);
#2163=VECTOR('',#7505,10.);
#2164=VECTOR('',#7506,10.);
#2165=VECTOR('',#7507,10.);
#2166=VECTOR('',#7508,10.);
#2167=VECTOR('',#7509,10.);
#2168=VECTOR('',#7510,10.);
#2169=VECTOR('',#7511,10.);
#2170=VECTOR('',#7514,10.);
#2171=VECTOR('',#7519,10.);
#2172=VECTOR('',#7522,10.);
#2173=VECTOR('',#7525,10.);
#2174=VECTOR('',#7526,10.);
#2175=VECTOR('',#7529,10.);
#2176=VECTOR('',#7532,10.);
#2177=VECTOR('',#7537,10.);
#2178=VECTOR('',#7540,10.);
#2179=VECTOR('',#7611,10.);
#2180=VECTOR('',#7612,10.);
#2181=VECTOR('',#7615,10.);
#2182=VECTOR('',#7616,10.);
#2183=VECTOR('',#7619,10.);
#2184=VECTOR('',#7620,10.);
#2185=VECTOR('',#7623,10.);
#2186=VECTOR('',#7624,10.);
#2187=VECTOR('',#7627,10.);
#2188=VECTOR('',#7628,10.);
#2189=VECTOR('',#7631,10.);
#2190=VECTOR('',#7632,10.);
#2191=VECTOR('',#7635,10.);
#2192=VECTOR('',#7636,10.);
#2193=VECTOR('',#7639,10.);
#2194=VECTOR('',#7640,10.);
#2195=VECTOR('',#7643,10.);
#2196=VECTOR('',#7644,10.);
#2197=VECTOR('',#7647,10.);
#2198=VECTOR('',#7648,10.);
#2199=VECTOR('',#7651,10.);
#2200=VECTOR('',#7652,10.);
#2201=VECTOR('',#7655,10.);
#2202=VECTOR('',#7656,10.);
#2203=VECTOR('',#7661,10.);
#2204=VECTOR('',#7662,10.);
#2205=VECTOR('',#7663,10.);
#2206=VECTOR('',#7664,10.);
#2207=VECTOR('',#7675,10.);
#2208=VECTOR('',#7676,10.);
#2209=VECTOR('',#7677,10.);
#2210=VECTOR('',#7678,10.);
#2211=VECTOR('',#7687,3.5);
#2212=VECTOR('',#7690,3.5);
#2213=VECTOR('',#7693,10.);
#2214=VECTOR('',#7694,10.);
#2215=VECTOR('',#7697,10.);
#2216=VECTOR('',#7700,10.);
#2217=VECTOR('',#7709,3.5);
#2218=VECTOR('',#7716,3.5);
#2219=VECTOR('',#7721,10.);
#2220=VECTOR('',#7722,10.);
#2221=VECTOR('',#7723,10.);
#2222=VECTOR('',#7724,10.);
#2223=VECTOR('',#7727,10.);
#2224=VECTOR('',#7728,10.);
#2225=VECTOR('',#7729,10.);
#2226=VECTOR('',#7732,10.);
#2227=VECTOR('',#7733,10.);
#2228=VECTOR('',#7734,10.);
#2229=VECTOR('',#7737,10.);
#2230=VECTOR('',#7738,10.);
#2231=VECTOR('',#7741,10.);
#2232=VECTOR('',#7742,10.);
#2233=VECTOR('',#7743,10.);
#2234=VECTOR('',#7744,10.);
#2235=VECTOR('',#7747,10.);
#2236=VECTOR('',#7748,10.);
#2237=VECTOR('',#7749,10.);
#2238=VECTOR('',#7752,10.);
#2239=VECTOR('',#7753,10.);
#2240=VECTOR('',#7754,10.);
#2241=VECTOR('',#7757,10.);
#2242=VECTOR('',#7758,10.);
#2243=VECTOR('',#7769,2.5);
#2244=VECTOR('',#7776,2.5);
#2245=VECTOR('',#7783,2.5);
#2246=VECTOR('',#7790,2.5);
#2247=VECTOR('',#7795,10.);
#2248=VECTOR('',#7796,10.);
#2249=VECTOR('',#7797,10.);
#2250=VECTOR('',#7798,10.);
#2251=VECTOR('',#7801,10.);
#2252=VECTOR('',#7802,10.);
#2253=VECTOR('',#7803,10.);
#2254=VECTOR('',#7806,10.);
#2255=VECTOR('',#7807,10.);
#2256=VECTOR('',#7808,10.);
#2257=VECTOR('',#7811,10.);
#2258=VECTOR('',#7812,10.);
#2259=VECTOR('',#7815,10.);
#2260=VECTOR('',#7816,10.);
#2261=VECTOR('',#7817,10.);
#2262=VECTOR('',#7818,10.);
#2263=VECTOR('',#7821,10.);
#2264=VECTOR('',#7822,10.);
#2265=VECTOR('',#7823,10.);
#2266=VECTOR('',#7826,10.);
#2267=VECTOR('',#7827,10.);
#2268=VECTOR('',#7828,10.);
#2269=VECTOR('',#7831,10.);
#2270=VECTOR('',#7832,10.);
#2271=VECTOR('',#7835,10.);
#2272=VECTOR('',#7836,10.);
#2273=VECTOR('',#7837,10.);
#2274=VECTOR('',#7838,10.);
#2275=VECTOR('',#7841,10.);
#2276=VECTOR('',#7842,10.);
#2277=VECTOR('',#7843,10.);
#2278=VECTOR('',#7846,10.);
#2279=VECTOR('',#7847,10.);
#2280=VECTOR('',#7848,10.);
#2281=VECTOR('',#7851,10.);
#2282=VECTOR('',#7852,10.);
#2283=VECTOR('',#7855,10.);
#2284=VECTOR('',#7856,10.);
#2285=VECTOR('',#7857,10.);
#2286=VECTOR('',#7858,10.);
#2287=VECTOR('',#7861,10.);
#2288=VECTOR('',#7862,10.);
#2289=VECTOR('',#7863,10.);
#2290=VECTOR('',#7866,10.);
#2291=VECTOR('',#7867,10.);
#2292=VECTOR('',#7868,10.);
#2293=VECTOR('',#7871,10.);
#2294=VECTOR('',#7872,10.);
#2295=VECTOR('',#7883,1.);
#2296=VECTOR('',#7888,10.);
#2297=VECTOR('',#7889,10.);
#2298=VECTOR('',#7890,10.);
#2299=VECTOR('',#7891,10.);
#2300=VECTOR('',#7894,10.);
#2301=VECTOR('',#7895,10.);
#2302=VECTOR('',#7896,10.);
#2303=VECTOR('',#7899,10.);
#2304=VECTOR('',#7900,10.);
#2305=VECTOR('',#7901,10.);
#2306=VECTOR('',#7904,10.);
#2307=VECTOR('',#7905,10.);
#2308=VECTOR('',#7916,1.);
#2309=VECTOR('',#7921,10.);
#2310=VECTOR('',#7922,10.);
#2311=VECTOR('',#7923,10.);
#2312=VECTOR('',#7924,10.);
#2313=VECTOR('',#7927,10.);
#2314=VECTOR('',#7928,10.);
#2315=VECTOR('',#7929,10.);
#2316=VECTOR('',#7932,10.);
#2317=VECTOR('',#7933,10.);
#2318=VECTOR('',#7934,10.);
#2319=VECTOR('',#7937,10.);
#2320=VECTOR('',#7938,10.);
#2321=VECTOR('',#7947,2.);
#2322=VECTOR('',#7952,2.);
#2323=VECTOR('',#7955,2.);
#2324=VECTOR('',#7958,2.);
#2325=VECTOR('',#7961,2.);
#2326=VECTOR('',#7964,2.);
#2327=VECTOR('',#7967,2.);
#2328=VECTOR('',#7970,2.);
#2329=VECTOR('',#7973,2.);
#2330=VECTOR('',#7976,2.);
#2331=VECTOR('',#7979,1.5555);
#2332=VECTOR('',#7984,1.5555);
#2333=VECTOR('',#7987,1.5555);
#2334=VECTOR('',#7990,1.5555);
#2335=VECTOR('',#7993,1.5555);
#2336=VECTOR('',#7996,1.5555);
#2337=VECTOR('',#7999,1.5555);
#2338=VECTOR('',#8002,1.5555);
#2339=VECTOR('',#8005,1.5555);
#2340=VECTOR('',#8008,1.5555);
#2341=VECTOR('',#8013,1.5);
#2342=VECTOR('',#8024,10.);
#2343=VECTOR('',#8025,10.);
#2344=VECTOR('',#8026,10.);
#2345=VECTOR('',#8027,10.);
#2346=VECTOR('',#8030,10.);
#2347=VECTOR('',#8031,10.);
#2348=VECTOR('',#8032,10.);
#2349=VECTOR('',#8035,10.);
#2350=VECTOR('',#8036,10.);
#2351=VECTOR('',#8037,10.);
#2352=VECTOR('',#8040,10.);
#2353=VECTOR('',#8041,10.);
#2354=VECTOR('',#8042,10.);
#2355=VECTOR('',#8045,10.);
#2356=VECTOR('',#8046,10.);
#2357=VECTOR('',#8047,10.);
#2358=VECTOR('',#8050,10.);
#2359=VECTOR('',#8051,10.);
#2360=VECTOR('',#8060,3.5);
#2361=VECTOR('',#8071,3.);
#2362=VECTOR('',#8076,3.);
#2363=VECTOR('',#8079,3.);
#2364=VECTOR('',#8082,3.);
#2365=VECTOR('',#8085,3.);
#2366=VECTOR('',#8088,3.);
#2367=VECTOR('',#8091,3.);
#2368=VECTOR('',#8094,3.);
#2369=VECTOR('',#8097,3.);
#2370=VECTOR('',#8100,3.);
#2371=VECTOR('',#8103,3.);
#2372=VECTOR('',#8106,3.);
#2373=VECTOR('',#8109,3.);
#2374=VECTOR('',#8112,3.);
#2375=VECTOR('',#8115,3.);
#2376=VECTOR('',#8118,2.37175);
#2377=VECTOR('',#8123,2.37175);
#2378=VECTOR('',#8126,2.37175);
#2379=VECTOR('',#8129,2.37175);
#2380=VECTOR('',#8132,2.37175);
#2381=VECTOR('',#8135,2.37175);
#2382=VECTOR('',#8138,2.37175);
#2383=VECTOR('',#8141,2.37175);
#2384=VECTOR('',#8144,2.37175);
#2385=VECTOR('',#8147,2.37175);
#2386=VECTOR('',#8150,2.37175);
#2387=VECTOR('',#8153,2.37175);
#2388=VECTOR('',#8156,2.37175);
#2389=VECTOR('',#8159,2.37175);
#2390=VECTOR('',#8162,2.37175);
#2391=VECTOR('',#8167,2.5);
#2392=VECTOR('',#8178,10.);
#2393=VECTOR('',#8179,10.);
#2394=VECTOR('',#8180,10.);
#2395=VECTOR('',#8181,10.);
#2396=VECTOR('',#8184,10.);
#2397=VECTOR('',#8185,10.);
#2398=VECTOR('',#8186,10.);
#2399=VECTOR('',#8189,10.);
#2400=VECTOR('',#8190,10.);
#2401=VECTOR('',#8191,10.);
#2402=VECTOR('',#8194,10.);
#2403=VECTOR('',#8195,10.);
#2404=VECTOR('',#8196,10.);
#2405=VECTOR('',#8199,10.);
#2406=VECTOR('',#8200,10.);
#2407=VECTOR('',#8201,10.);
#2408=VECTOR('',#8204,10.);
#2409=VECTOR('',#8205,10.);
#2410=VECTOR('',#8214,5.);
#2411=VECTOR('',#8227,3.5);
#2412=VECTOR('',#8234,7.);
#2413=VECTOR('',#8245,3.);
#2414=VECTOR('',#8250,3.);
#2415=VECTOR('',#8253,3.);
#2416=VECTOR('',#8256,3.);
#2417=VECTOR('',#8259,3.);
#2418=VECTOR('',#8264,3.0735);
#2419=VECTOR('',#8269,3.0735);
#2420=VECTOR('',#8272,3.0735);
#2421=VECTOR('',#8275,3.0735);
#2422=VECTOR('',#8278,3.0735);
#2423=VECTOR('',#8285,10.);
#2424=VECTOR('',#8286,10.);
#2425=VECTOR('',#8287,10.);
#2426=VECTOR('',#8288,10.);
#2427=VECTOR('',#8289,10.);
#2428=VECTOR('',#8290,10.);
#2429=VECTOR('',#8295,10.);
#2430=VECTOR('',#8296,10.);
#2431=VECTOR('',#8297,10.);
#2432=VECTOR('',#8300,10.);
#2433=VECTOR('',#8301,10.);
#2434=VECTOR('',#8304,10.);
#2435=VECTOR('',#8305,10.);
#2436=VECTOR('',#8308,10.);
#2437=VECTOR('',#8309,10.);
#2438=VECTOR('',#8312,10.);
#2439=VECTOR('',#8313,10.);
#2440=VECTOR('',#8316,10.);
#2441=VERTEX_POINT('',#8356);
#2442=VERTEX_POINT('',#8357);
#2443=VERTEX_POINT('',#8359);
#2444=VERTEX_POINT('',#8373);
#2445=VERTEX_POINT('',#8395);
#2446=VERTEX_POINT('',#8396);
#2447=VERTEX_POINT('',#8443);
#2448=VERTEX_POINT('',#8444);
#2449=VERTEX_POINT('',#8491);
#2450=VERTEX_POINT('',#8492);
#2451=VERTEX_POINT('',#8542);
#2452=VERTEX_POINT('',#8543);
#2453=VERTEX_POINT('',#8590);
#2454=VERTEX_POINT('',#8591);
#2455=VERTEX_POINT('',#8638);
#2456=VERTEX_POINT('',#8639);
#2457=VERTEX_POINT('',#8689);
#2458=VERTEX_POINT('',#8690);
#2459=VERTEX_POINT('',#8740);
#2460=VERTEX_POINT('',#8741);
#2461=VERTEX_POINT('',#8788);
#2462=VERTEX_POINT('',#8789);
#2463=VERTEX_POINT('',#8839);
#2464=VERTEX_POINT('',#8840);
#2465=VERTEX_POINT('',#8842);
#2466=VERTEX_POINT('',#8856);
#2467=VERTEX_POINT('',#8878);
#2468=VERTEX_POINT('',#8879);
#2469=VERTEX_POINT('',#8881);
#2470=VERTEX_POINT('',#8895);
#2471=VERTEX_POINT('',#8917);
#2472=VERTEX_POINT('',#8918);
#2473=VERTEX_POINT('',#8965);
#2474=VERTEX_POINT('',#8966);
#2475=VERTEX_POINT('',#9013);
#2476=VERTEX_POINT('',#9014);
#2477=VERTEX_POINT('',#9064);
#2478=VERTEX_POINT('',#9065);
#2479=VERTEX_POINT('',#9112);
#2480=VERTEX_POINT('',#9113);
#2481=VERTEX_POINT('',#9160);
#2482=VERTEX_POINT('',#9161);
#2483=VERTEX_POINT('',#9211);
#2484=VERTEX_POINT('',#9212);
#2485=VERTEX_POINT('',#9262);
#2486=VERTEX_POINT('',#9263);
#2487=VERTEX_POINT('',#9310);
#2488=VERTEX_POINT('',#9311);
#2489=VERTEX_POINT('',#9361);
#2490=VERTEX_POINT('',#9362);
#2491=VERTEX_POINT('',#9364);
#2492=VERTEX_POINT('',#9378);
#2493=VERTEX_POINT('',#9400);
#2494=VERTEX_POINT('',#9401);
#2495=VERTEX_POINT('',#9403);
#2496=VERTEX_POINT('',#9417);
#2497=VERTEX_POINT('',#9439);
#2498=VERTEX_POINT('',#9440);
#2499=VERTEX_POINT('',#9487);
#2500=VERTEX_POINT('',#9488);
#2501=VERTEX_POINT('',#9535);
#2502=VERTEX_POINT('',#9536);
#2503=VERTEX_POINT('',#9586);
#2504=VERTEX_POINT('',#9587);
#2505=VERTEX_POINT('',#9634);
#2506=VERTEX_POINT('',#9635);
#2507=VERTEX_POINT('',#9682);
#2508=VERTEX_POINT('',#9683);
#2509=VERTEX_POINT('',#9733);
#2510=VERTEX_POINT('',#9734);
#2511=VERTEX_POINT('',#9784);
#2512=VERTEX_POINT('',#9785);
#2513=VERTEX_POINT('',#9832);
#2514=VERTEX_POINT('',#9833);
#2515=VERTEX_POINT('',#9883);
#2516=VERTEX_POINT('',#9884);
#2517=VERTEX_POINT('',#9886);
#2518=VERTEX_POINT('',#9900);
#2519=VERTEX_POINT('',#9902);
#2520=VERTEX_POINT('',#9924);
#2521=VERTEX_POINT('',#9925);
#2522=VERTEX_POINT('',#9927);
#2523=VERTEX_POINT('',#9941);
#2524=VERTEX_POINT('',#9963);
#2525=VERTEX_POINT('',#9964);
#2526=VERTEX_POINT('',#10011);
#2527=VERTEX_POINT('',#10012);
#2528=VERTEX_POINT('',#10059);
#2529=VERTEX_POINT('',#10060);
#2530=VERTEX_POINT('',#10110);
#2531=VERTEX_POINT('',#10111);
#2532=VERTEX_POINT('',#10158);
#2533=VERTEX_POINT('',#10159);
#2534=VERTEX_POINT('',#10206);
#2535=VERTEX_POINT('',#10207);
#2536=VERTEX_POINT('',#10257);
#2537=VERTEX_POINT('',#10258);
#2538=VERTEX_POINT('',#10308);
#2539=VERTEX_POINT('',#10309);
#2540=VERTEX_POINT('',#10356);
#2541=VERTEX_POINT('',#10357);
#2542=VERTEX_POINT('',#10407);
#2543=VERTEX_POINT('',#10408);
#2544=VERTEX_POINT('',#10410);
#2545=VERTEX_POINT('',#10424);
#2546=VERTEX_POINT('',#10426);
#2547=VERTEX_POINT('',#10448);
#2548=VERTEX_POINT('',#10449);
#2549=VERTEX_POINT('',#10451);
#2550=VERTEX_POINT('',#10456);
#2551=VERTEX_POINT('',#10464);
#2552=VERTEX_POINT('',#10465);
#2553=VERTEX_POINT('',#10489);
#2554=VERTEX_POINT('',#10490);
#2555=VERTEX_POINT('',#10514);
#2556=VERTEX_POINT('',#10515);
#2557=VERTEX_POINT('',#10538);
#2558=VERTEX_POINT('',#10539);
#2559=VERTEX_POINT('',#10563);
#2560=VERTEX_POINT('',#10564);
#2561=VERTEX_POINT('',#10587);
#2562=VERTEX_POINT('',#10588);
#2563=VERTEX_POINT('',#10612);
#2564=VERTEX_POINT('',#10613);
#2565=VERTEX_POINT('',#10636);
#2566=VERTEX_POINT('',#10637);
#2567=VERTEX_POINT('',#10661);
#2568=VERTEX_POINT('',#10662);
#2569=VERTEX_POINT('',#10686);
#2570=VERTEX_POINT('',#10687);
#2571=VERTEX_POINT('',#10710);
#2572=VERTEX_POINT('',#10711);
#2573=VERTEX_POINT('',#10713);
#2574=VERTEX_POINT('',#10719);
#2575=VERTEX_POINT('',#10727);
#2576=VERTEX_POINT('',#10728);
#2577=VERTEX_POINT('',#10730);
#2578=VERTEX_POINT('',#10735);
#2579=VERTEX_POINT('',#10743);
#2580=VERTEX_POINT('',#10744);
#2581=VERTEX_POINT('',#10768);
#2582=VERTEX_POINT('',#10769);
#2583=VERTEX_POINT('',#10793);
#2584=VERTEX_POINT('',#10794);
#2585=VERTEX_POINT('',#10817);
#2586=VERTEX_POINT('',#10818);
#2587=VERTEX_POINT('',#10842);
#2588=VERTEX_POINT('',#10843);
#2589=VERTEX_POINT('',#10866);
#2590=VERTEX_POINT('',#10867);
#2591=VERTEX_POINT('',#10891);
#2592=VERTEX_POINT('',#10892);
#2593=VERTEX_POINT('',#10915);
#2594=VERTEX_POINT('',#10916);
#2595=VERTEX_POINT('',#10940);
#2596=VERTEX_POINT('',#10941);
#2597=VERTEX_POINT('',#10965);
#2598=VERTEX_POINT('',#10966);
#2599=VERTEX_POINT('',#10989);
#2600=VERTEX_POINT('',#10990);
#2601=VERTEX_POINT('',#10992);
#2602=VERTEX_POINT('',#10998);
#2603=VERTEX_POINT('',#11006);
#2604=VERTEX_POINT('',#11007);
#2605=VERTEX_POINT('',#11009);
#2606=VERTEX_POINT('',#11014);
#2607=VERTEX_POINT('',#11022);
#2608=VERTEX_POINT('',#11023);
#2609=VERTEX_POINT('',#11047);
#2610=VERTEX_POINT('',#11048);
#2611=VERTEX_POINT('',#11072);
#2612=VERTEX_POINT('',#11073);
#2613=VERTEX_POINT('',#11096);
#2614=VERTEX_POINT('',#11097);
#2615=VERTEX_POINT('',#11121);
#2616=VERTEX_POINT('',#11122);
#2617=VERTEX_POINT('',#11145);
#2618=VERTEX_POINT('',#11146);
#2619=VERTEX_POINT('',#11170);
#2620=VERTEX_POINT('',#11171);
#2621=VERTEX_POINT('',#11194);
#2622=VERTEX_POINT('',#11195);
#2623=VERTEX_POINT('',#11219);
#2624=VERTEX_POINT('',#11220);
#2625=VERTEX_POINT('',#11244);
#2626=VERTEX_POINT('',#11245);
#2627=VERTEX_POINT('',#11268);
#2628=VERTEX_POINT('',#11269);
#2629=VERTEX_POINT('',#11271);
#2630=VERTEX_POINT('',#11277);
#2631=VERTEX_POINT('',#11285);
#2632=VERTEX_POINT('',#11286);
#2633=VERTEX_POINT('',#11288);
#2634=VERTEX_POINT('',#11293);
#2635=VERTEX_POINT('',#11301);
#2636=VERTEX_POINT('',#11302);
#2637=VERTEX_POINT('',#11326);
#2638=VERTEX_POINT('',#11327);
#2639=VERTEX_POINT('',#11351);
#2640=VERTEX_POINT('',#11352);
#2641=VERTEX_POINT('',#11375);
#2642=VERTEX_POINT('',#11376);
#2643=VERTEX_POINT('',#11400);
#2644=VERTEX_POINT('',#11401);
#2645=VERTEX_POINT('',#11424);
#2646=VERTEX_POINT('',#11425);
#2647=VERTEX_POINT('',#11449);
#2648=VERTEX_POINT('',#11450);
#2649=VERTEX_POINT('',#11473);
#2650=VERTEX_POINT('',#11474);
#2651=VERTEX_POINT('',#11498);
#2652=VERTEX_POINT('',#11499);
#2653=VERTEX_POINT('',#11523);
#2654=VERTEX_POINT('',#11524);
#2655=VERTEX_POINT('',#11547);
#2656=VERTEX_POINT('',#11548);
#2657=VERTEX_POINT('',#11550);
#2658=VERTEX_POINT('',#11556);
#2659=VERTEX_POINT('',#11564);
#2660=VERTEX_POINT('',#11565);
#2661=VERTEX_POINT('',#11567);
#2662=VERTEX_POINT('',#11569);
#2663=VERTEX_POINT('',#11573);
#2664=VERTEX_POINT('',#11575);
#2665=VERTEX_POINT('',#11579);
#2666=VERTEX_POINT('',#11581);
#2667=VERTEX_POINT('',#11585);
#2668=VERTEX_POINT('',#11587);
#2669=VERTEX_POINT('',#11591);
#2670=VERTEX_POINT('',#11593);
#2671=VERTEX_POINT('',#11600);
#2672=VERTEX_POINT('',#11602);
#2673=VERTEX_POINT('',#11604);
#2674=VERTEX_POINT('',#11606);
#2675=VERTEX_POINT('',#11610);
#2676=VERTEX_POINT('',#11615);
#2677=VERTEX_POINT('',#11619);
#2678=VERTEX_POINT('',#11620);
#2679=VERTEX_POINT('',#11622);
#2680=VERTEX_POINT('',#11624);
#2681=VERTEX_POINT('',#11626);
#2682=VERTEX_POINT('',#11628);
#2683=VERTEX_POINT('',#11630);
#2684=VERTEX_POINT('',#11632);
#2685=VERTEX_POINT('',#11634);
#2686=VERTEX_POINT('',#11638);
#2687=VERTEX_POINT('',#11659);
#2688=VERTEX_POINT('',#11661);
#2689=VERTEX_POINT('',#11665);
#2690=VERTEX_POINT('',#11687);
#2691=VERTEX_POINT('',#11693);
#2692=VERTEX_POINT('',#11695);
#2693=VERTEX_POINT('',#11699);
#2694=VERTEX_POINT('',#11703);
#2695=VERTEX_POINT('',#11705);
#2696=VERTEX_POINT('',#11709);
#2697=VERTEX_POINT('',#11711);
#2698=VERTEX_POINT('',#11715);
#2699=VERTEX_POINT('',#11719);
#2700=VERTEX_POINT('',#12746);
#2701=VERTEX_POINT('',#12747);
#2702=VERTEX_POINT('',#12749);
#2703=VERTEX_POINT('',#12751);
#2704=VERTEX_POINT('',#12753);
#2705=VERTEX_POINT('',#12755);
#2706=VERTEX_POINT('',#12758);
#2707=VERTEX_POINT('',#12759);
#2708=VERTEX_POINT('',#12761);
#2709=VERTEX_POINT('',#12763);
#2710=VERTEX_POINT('',#12766);
#2711=VERTEX_POINT('',#12767);
#2712=VERTEX_POINT('',#12769);
#2713=VERTEX_POINT('',#12771);
#2714=VERTEX_POINT('',#12774);
#2715=VERTEX_POINT('',#12775);
#2716=VERTEX_POINT('',#12777);
#2717=VERTEX_POINT('',#12779);
#2718=VERTEX_POINT('',#15862);
#2719=VERTEX_POINT('',#15864);
#2720=VERTEX_POINT('',#15867);
#2721=VERTEX_POINT('',#15868);
#2722=VERTEX_POINT('',#15870);
#2723=VERTEX_POINT('',#15872);
#2724=VERTEX_POINT('',#15875);
#2725=VERTEX_POINT('',#15876);
#2726=VERTEX_POINT('',#15878);
#2727=VERTEX_POINT('',#15880);
#2728=VERTEX_POINT('',#15883);
#2729=VERTEX_POINT('',#15884);
#2730=VERTEX_POINT('',#15886);
#2731=VERTEX_POINT('',#15888);
#2732=VERTEX_POINT('',#15925);
#2733=VERTEX_POINT('',#15928);
#2734=VERTEX_POINT('',#15929);
#2735=VERTEX_POINT('',#15931);
#2736=VERTEX_POINT('',#15933);
#2737=VERTEX_POINT('',#15935);
#2738=VERTEX_POINT('',#15937);
#2739=VERTEX_POINT('',#15962);
#2740=VERTEX_POINT('',#15963);
#2741=VERTEX_POINT('',#15965);
#2742=VERTEX_POINT('',#15969);
#2743=VERTEX_POINT('',#15970);
#2744=VERTEX_POINT('',#15972);
#2745=VERTEX_POINT('',#15976);
#2746=VERTEX_POINT('',#15977);
#2747=VERTEX_POINT('',#15979);
#2748=VERTEX_POINT('',#15983);
#2749=VERTEX_POINT('',#15984);
#2750=VERTEX_POINT('',#15986);
#2751=VERTEX_POINT('',#15990);
#2752=VERTEX_POINT('',#15991);
#2753=VERTEX_POINT('',#15993);
#2754=VERTEX_POINT('',#15997);
#2755=VERTEX_POINT('',#15998);
#2756=VERTEX_POINT('',#16000);
#2757=VERTEX_POINT('',#16004);
#2758=VERTEX_POINT('',#16005);
#2759=VERTEX_POINT('',#16007);
#2760=VERTEX_POINT('',#16011);
#2761=VERTEX_POINT('',#16012);
#2762=VERTEX_POINT('',#16014);
#2763=VERTEX_POINT('',#16055);
#2764=VERTEX_POINT('',#16056);
#2765=VERTEX_POINT('',#16058);
#2766=VERTEX_POINT('',#16060);
#2767=VERTEX_POINT('',#16063);
#2768=VERTEX_POINT('',#16065);
#2769=VERTEX_POINT('',#16070);
#2770=VERTEX_POINT('',#16071);
#2771=VERTEX_POINT('',#16073);
#2772=VERTEX_POINT('',#16075);
#2773=VERTEX_POINT('',#16078);
#2774=VERTEX_POINT('',#16080);
#2775=VERTEX_POINT('',#16097);
#2776=VERTEX_POINT('',#16099);
#2777=VERTEX_POINT('',#16103);
#2778=VERTEX_POINT('',#16105);
#2779=VERTEX_POINT('',#16109);
#2780=VERTEX_POINT('',#16110);
#2781=VERTEX_POINT('',#16112);
#2782=VERTEX_POINT('',#16114);
#2783=VERTEX_POINT('',#16118);
#2784=VERTEX_POINT('',#16120);
#2785=VERTEX_POINT('',#16124);
#2786=VERTEX_POINT('',#16126);
#2787=VERTEX_POINT('',#16133);
#2788=VERTEX_POINT('',#16134);
#2789=VERTEX_POINT('',#16136);
#2790=VERTEX_POINT('',#16138);
#2791=VERTEX_POINT('',#16142);
#2792=VERTEX_POINT('',#16144);
#2793=VERTEX_POINT('',#16148);
#2794=VERTEX_POINT('',#16150);
#2795=VERTEX_POINT('',#16160);
#2796=VERTEX_POINT('',#16162);
#2797=VERTEX_POINT('',#16166);
#2798=VERTEX_POINT('',#16168);
#2799=VERTEX_POINT('',#16172);
#2800=VERTEX_POINT('',#16174);
#2801=VERTEX_POINT('',#16178);
#2802=VERTEX_POINT('',#16180);
#2803=VERTEX_POINT('',#16184);
#2804=VERTEX_POINT('',#16185);
#2805=VERTEX_POINT('',#16187);
#2806=VERTEX_POINT('',#16189);
#2807=VERTEX_POINT('',#16193);
#2808=VERTEX_POINT('',#16195);
#2809=VERTEX_POINT('',#16199);
#2810=VERTEX_POINT('',#16201);
#2811=VERTEX_POINT('',#16208);
#2812=VERTEX_POINT('',#16209);
#2813=VERTEX_POINT('',#16211);
#2814=VERTEX_POINT('',#16213);
#2815=VERTEX_POINT('',#16217);
#2816=VERTEX_POINT('',#16219);
#2817=VERTEX_POINT('',#16223);
#2818=VERTEX_POINT('',#16225);
#2819=VERTEX_POINT('',#16232);
#2820=VERTEX_POINT('',#16233);
#2821=VERTEX_POINT('',#16235);
#2822=VERTEX_POINT('',#16237);
#2823=VERTEX_POINT('',#16241);
#2824=VERTEX_POINT('',#16243);
#2825=VERTEX_POINT('',#16247);
#2826=VERTEX_POINT('',#16249);
#2827=VERTEX_POINT('',#16256);
#2828=VERTEX_POINT('',#16257);
#2829=VERTEX_POINT('',#16259);
#2830=VERTEX_POINT('',#16261);
#2831=VERTEX_POINT('',#16265);
#2832=VERTEX_POINT('',#16267);
#2833=VERTEX_POINT('',#16271);
#2834=VERTEX_POINT('',#16273);
#2835=VERTEX_POINT('',#16283);
#2836=VERTEX_POINT('',#16285);
#2837=VERTEX_POINT('',#16289);
#2838=VERTEX_POINT('',#16290);
#2839=VERTEX_POINT('',#16292);
#2840=VERTEX_POINT('',#16294);
#2841=VERTEX_POINT('',#16298);
#2842=VERTEX_POINT('',#16300);
#2843=VERTEX_POINT('',#16304);
#2844=VERTEX_POINT('',#16306);
#2845=VERTEX_POINT('',#16316);
#2846=VERTEX_POINT('',#16318);
#2847=VERTEX_POINT('',#16322);
#2848=VERTEX_POINT('',#16323);
#2849=VERTEX_POINT('',#16325);
#2850=VERTEX_POINT('',#16327);
#2851=VERTEX_POINT('',#16331);
#2852=VERTEX_POINT('',#16333);
#2853=VERTEX_POINT('',#16337);
#2854=VERTEX_POINT('',#16339);
#2855=VERTEX_POINT('',#16349);
#2856=VERTEX_POINT('',#16350);
#2857=VERTEX_POINT('',#16352);
#2858=VERTEX_POINT('',#16363);
#2859=VERTEX_POINT('',#16373);
#2860=VERTEX_POINT('',#16374);
#2861=VERTEX_POINT('',#16421);
#2862=VERTEX_POINT('',#16422);
#2863=VERTEX_POINT('',#16469);
#2864=VERTEX_POINT('',#16470);
#2865=VERTEX_POINT('',#16520);
#2866=VERTEX_POINT('',#16521);
#2867=VERTEX_POINT('',#16571);
#2868=VERTEX_POINT('',#16572);
#2869=VERTEX_POINT('',#16619);
#2870=VERTEX_POINT('',#16620);
#2871=VERTEX_POINT('',#16667);
#2872=VERTEX_POINT('',#16668);
#2873=VERTEX_POINT('',#16721);
#2874=VERTEX_POINT('',#16722);
#2875=VERTEX_POINT('',#16769);
#2876=VERTEX_POINT('',#16770);
#2877=VERTEX_POINT('',#16817);
#2878=VERTEX_POINT('',#16818);
#2879=VERTEX_POINT('',#16820);
#2880=VERTEX_POINT('',#16831);
#2881=VERTEX_POINT('',#16842);
#2882=VERTEX_POINT('',#16843);
#2883=VERTEX_POINT('',#16867);
#2884=VERTEX_POINT('',#16868);
#2885=VERTEX_POINT('',#16891);
#2886=VERTEX_POINT('',#16892);
#2887=VERTEX_POINT('',#16916);
#2888=VERTEX_POINT('',#16917);
#2889=VERTEX_POINT('',#16941);
#2890=VERTEX_POINT('',#16942);
#2891=VERTEX_POINT('',#16965);
#2892=VERTEX_POINT('',#16966);
#2893=VERTEX_POINT('',#16989);
#2894=VERTEX_POINT('',#16990);
#2895=VERTEX_POINT('',#17015);
#2896=VERTEX_POINT('',#17016);
#2897=VERTEX_POINT('',#17039);
#2898=VERTEX_POINT('',#17040);
#2899=VERTEX_POINT('',#17063);
#2900=VERTEX_POINT('',#17269);
#2901=VERTEX_POINT('',#17328);
#2902=VERTEX_POINT('',#17358);
#2903=VERTEX_POINT('',#17641);
#2904=VERTEX_POINT('',#17755);
#2905=VERTEX_POINT('',#18160);
#2906=VERTEX_POINT('',#18161);
#2907=VERTEX_POINT('',#18163);
#2908=VERTEX_POINT('',#18165);
#2909=VERTEX_POINT('',#18169);
#2910=VERTEX_POINT('',#18171);
#2911=VERTEX_POINT('',#18175);
#2912=VERTEX_POINT('',#18177);
#2913=VERTEX_POINT('',#18181);
#2914=VERTEX_POINT('',#18183);
#2915=VERTEX_POINT('',#18187);
#2916=VERTEX_POINT('',#18189);
#2917=VERTEX_POINT('',#18197);
#2918=VERTEX_POINT('',#18200);
#2919=VERTEX_POINT('',#18207);
#2920=VERTEX_POINT('',#18208);
#2921=VERTEX_POINT('',#18210);
#2922=VERTEX_POINT('',#18221);
#2923=VERTEX_POINT('',#18231);
#2924=VERTEX_POINT('',#18232);
#2925=VERTEX_POINT('',#18279);
#2926=VERTEX_POINT('',#18280);
#2927=VERTEX_POINT('',#18327);
#2928=VERTEX_POINT('',#18328);
#2929=VERTEX_POINT('',#18381);
#2930=VERTEX_POINT('',#18382);
#2931=VERTEX_POINT('',#18429);
#2932=VERTEX_POINT('',#18430);
#2933=VERTEX_POINT('',#18477);
#2934=VERTEX_POINT('',#18478);
#2935=VERTEX_POINT('',#18531);
#2936=VERTEX_POINT('',#18532);
#2937=VERTEX_POINT('',#18579);
#2938=VERTEX_POINT('',#18580);
#2939=VERTEX_POINT('',#18627);
#2940=VERTEX_POINT('',#18628);
#2941=VERTEX_POINT('',#18681);
#2942=VERTEX_POINT('',#18682);
#2943=VERTEX_POINT('',#18729);
#2944=VERTEX_POINT('',#18730);
#2945=VERTEX_POINT('',#18777);
#2946=VERTEX_POINT('',#18778);
#2947=VERTEX_POINT('',#18831);
#2948=VERTEX_POINT('',#18832);
#2949=VERTEX_POINT('',#18879);
#2950=VERTEX_POINT('',#18880);
#2951=VERTEX_POINT('',#18927);
#2952=VERTEX_POINT('',#18928);
#2953=VERTEX_POINT('',#18930);
#2954=VERTEX_POINT('',#18941);
#2955=VERTEX_POINT('',#18952);
#2956=VERTEX_POINT('',#18953);
#2957=VERTEX_POINT('',#18977);
#2958=VERTEX_POINT('',#18978);
#2959=VERTEX_POINT('',#19001);
#2960=VERTEX_POINT('',#19002);
#2961=VERTEX_POINT('',#19026);
#2962=VERTEX_POINT('',#19027);
#2963=VERTEX_POINT('',#19051);
#2964=VERTEX_POINT('',#19052);
#2965=VERTEX_POINT('',#19075);
#2966=VERTEX_POINT('',#19076);
#2967=VERTEX_POINT('',#19100);
#2968=VERTEX_POINT('',#19101);
#2969=VERTEX_POINT('',#19125);
#2970=VERTEX_POINT('',#19126);
#2971=VERTEX_POINT('',#19149);
#2972=VERTEX_POINT('',#19150);
#2973=VERTEX_POINT('',#19174);
#2974=VERTEX_POINT('',#19175);
#2975=VERTEX_POINT('',#19199);
#2976=VERTEX_POINT('',#19200);
#2977=VERTEX_POINT('',#19223);
#2978=VERTEX_POINT('',#19224);
#2979=VERTEX_POINT('',#19248);
#2980=VERTEX_POINT('',#19249);
#2981=VERTEX_POINT('',#19273);
#2982=VERTEX_POINT('',#19274);
#2983=VERTEX_POINT('',#19297);
#2984=VERTEX_POINT('',#19518);
#2985=VERTEX_POINT('',#19583);
#2986=VERTEX_POINT('',#19616);
#2987=VERTEX_POINT('',#20027);
#2988=VERTEX_POINT('',#20144);
#2989=VERTEX_POINT('',#20683);
#2990=VERTEX_POINT('',#20684);
#2991=VERTEX_POINT('',#20686);
#2992=VERTEX_POINT('',#20688);
#2993=VERTEX_POINT('',#20692);
#2994=VERTEX_POINT('',#20694);
#2995=VERTEX_POINT('',#20698);
#2996=VERTEX_POINT('',#20700);
#2997=VERTEX_POINT('',#20704);
#2998=VERTEX_POINT('',#20706);
#2999=VERTEX_POINT('',#20710);
#3000=VERTEX_POINT('',#20712);
#3001=VERTEX_POINT('',#20720);
#3002=VERTEX_POINT('',#20723);
#3003=VERTEX_POINT('',#20730);
#3004=VERTEX_POINT('',#20732);
#3005=VERTEX_POINT('',#20736);
#3006=VERTEX_POINT('',#20738);
#3007=VERTEX_POINT('',#20745);
#3008=VERTEX_POINT('',#20746);
#3009=VERTEX_POINT('',#20748);
#3010=VERTEX_POINT('',#20753);
#3011=VERTEX_POINT('',#20766);
#3012=VERTEX_POINT('',#20767);
#3013=VERTEX_POINT('',#20817);
#3014=VERTEX_POINT('',#20818);
#3015=VERTEX_POINT('',#20868);
#3016=VERTEX_POINT('',#20869);
#3017=VERTEX_POINT('',#20916);
#3018=VERTEX_POINT('',#20917);
#3019=VERTEX_POINT('',#20919);
#3020=VERTEX_POINT('',#20933);
#3021=VERTEX_POINT('',#20955);
#3022=VERTEX_POINT('',#20956);
#3023=VERTEX_POINT('',#20958);
#3024=VERTEX_POINT('',#20967);
#3025=VERTEX_POINT('',#20979);
#3026=VERTEX_POINT('',#20980);
#3027=VERTEX_POINT('',#21003);
#3028=VERTEX_POINT('',#21004);
#3029=VERTEX_POINT('',#21028);
#3030=VERTEX_POINT('',#21029);
#3031=VERTEX_POINT('',#21053);
#3032=VERTEX_POINT('',#21054);
#3033=VERTEX_POINT('',#21056);
#3034=VERTEX_POINT('',#21062);
#3035=VERTEX_POINT('',#21802);
#3036=VERTEX_POINT('',#21803);
#3037=VERTEX_POINT('',#21805);
#3038=VERTEX_POINT('',#21807);
#3039=VERTEX_POINT('',#21809);
#3040=VERTEX_POINT('',#21811);
#3041=VERTEX_POINT('',#21816);
#3042=VERTEX_POINT('',#21817);
#3043=VERTEX_POINT('',#21822);
#3044=VERTEX_POINT('',#21826);
#3045=VERTEX_POINT('',#21830);
#3046=VERTEX_POINT('',#21834);
#3047=EDGE_CURVE('',#2441,#2442,#1529,.T.);
#3048=EDGE_CURVE('',#2442,#2443,#1162,.T.);
#3049=EDGE_CURVE('',#2444,#2443,#1067,.F.);
#3050=EDGE_CURVE('',#2444,#2441,#1163,.T.);
#3051=EDGE_CURVE('',#2445,#2446,#1530,.T.);
#3052=EDGE_CURVE('',#2446,#2442,#1164,.T.);
#3053=EDGE_CURVE('',#2441,#2445,#1165,.T.);
#3054=EDGE_CURVE('',#2447,#2448,#1531,.T.);
#3055=EDGE_CURVE('',#2448,#2446,#1166,.T.);
#3056=EDGE_CURVE('',#2445,#2447,#1167,.T.);
#3057=EDGE_CURVE('',#2449,#2450,#1532,.T.);
#3058=EDGE_CURVE('',#2450,#2448,#1168,.T.);
#3059=EDGE_CURVE('',#2447,#2449,#1169,.T.);
#3060=EDGE_CURVE('',#2451,#2452,#1533,.T.);
#3061=EDGE_CURVE('',#2452,#2450,#1170,.T.);
#3062=EDGE_CURVE('',#2449,#2451,#1171,.T.);
#3063=EDGE_CURVE('',#2453,#2454,#1534,.T.);
#3064=EDGE_CURVE('',#2454,#2452,#1172,.T.);
#3065=EDGE_CURVE('',#2451,#2453,#1173,.T.);
#3066=EDGE_CURVE('',#2455,#2456,#1535,.T.);
#3067=EDGE_CURVE('',#2456,#2454,#1174,.T.);
#3068=EDGE_CURVE('',#2453,#2455,#1175,.T.);
#3069=EDGE_CURVE('',#2457,#2458,#1536,.T.);
#3070=EDGE_CURVE('',#2458,#2456,#1176,.T.);
#3071=EDGE_CURVE('',#2455,#2457,#1177,.T.);
#3072=EDGE_CURVE('',#2459,#2460,#1537,.T.);
#3073=EDGE_CURVE('',#2460,#2458,#1178,.T.);
#3074=EDGE_CURVE('',#2457,#2459,#1179,.T.);
#3075=EDGE_CURVE('',#2461,#2462,#1538,.T.);
#3076=EDGE_CURVE('',#2462,#2460,#1180,.T.);
#3077=EDGE_CURVE('',#2459,#2461,#1181,.T.);
#3078=EDGE_CURVE('',#2463,#2464,#1539,.T.);
#3079=EDGE_CURVE('',#2463,#2465,#1182,.T.);
#3080=EDGE_CURVE('',#2465,#2466,#1068,.F.);
#3081=EDGE_CURVE('',#2466,#2464,#1183,.T.);
#3082=EDGE_CURVE('',#2467,#2468,#1540,.T.);
#3083=EDGE_CURVE('',#2468,#2469,#1184,.T.);
#3084=EDGE_CURVE('',#2470,#2469,#1069,.F.);
#3085=EDGE_CURVE('',#2470,#2467,#1185,.T.);
#3086=EDGE_CURVE('',#2471,#2472,#1541,.T.);
#3087=EDGE_CURVE('',#2472,#2468,#1186,.T.);
#3088=EDGE_CURVE('',#2467,#2471,#1187,.T.);
#3089=EDGE_CURVE('',#2473,#2474,#1542,.T.);
#3090=EDGE_CURVE('',#2474,#2472,#1188,.T.);
#3091=EDGE_CURVE('',#2471,#2473,#1189,.T.);
#3092=EDGE_CURVE('',#2475,#2476,#1543,.T.);
#3093=EDGE_CURVE('',#2476,#2474,#1190,.T.);
#3094=EDGE_CURVE('',#2473,#2475,#1191,.T.);
#3095=EDGE_CURVE('',#2477,#2478,#1544,.T.);
#3096=EDGE_CURVE('',#2478,#2476,#1192,.T.);
#3097=EDGE_CURVE('',#2475,#2477,#1193,.T.);
#3098=EDGE_CURVE('',#2479,#2480,#1545,.T.);
#3099=EDGE_CURVE('',#2480,#2478,#1194,.T.);
#3100=EDGE_CURVE('',#2477,#2479,#1195,.T.);
#3101=EDGE_CURVE('',#2481,#2482,#1546,.T.);
#3102=EDGE_CURVE('',#2482,#2480,#1196,.T.);
#3103=EDGE_CURVE('',#2479,#2481,#1197,.T.);
#3104=EDGE_CURVE('',#2483,#2484,#1547,.T.);
#3105=EDGE_CURVE('',#2484,#2482,#1198,.T.);
#3106=EDGE_CURVE('',#2481,#2483,#1199,.T.);
#3107=EDGE_CURVE('',#2485,#2486,#1548,.T.);
#3108=EDGE_CURVE('',#2486,#2484,#1200,.T.);
#3109=EDGE_CURVE('',#2483,#2485,#1201,.T.);
#3110=EDGE_CURVE('',#2487,#2488,#1549,.T.);
#3111=EDGE_CURVE('',#2488,#2486,#1202,.T.);
#3112=EDGE_CURVE('',#2485,#2487,#1203,.T.);
#3113=EDGE_CURVE('',#2489,#2490,#1550,.T.);
#3114=EDGE_CURVE('',#2489,#2491,#1204,.T.);
#3115=EDGE_CURVE('',#2491,#2492,#1070,.F.);
#3116=EDGE_CURVE('',#2492,#2490,#1205,.T.);
#3117=EDGE_CURVE('',#2493,#2494,#1551,.T.);
#3118=EDGE_CURVE('',#2494,#2495,#1206,.T.);
#3119=EDGE_CURVE('',#2496,#2495,#1071,.F.);
#3120=EDGE_CURVE('',#2496,#2493,#1207,.T.);
#3121=EDGE_CURVE('',#2497,#2498,#1552,.T.);
#3122=EDGE_CURVE('',#2498,#2494,#1208,.T.);
#3123=EDGE_CURVE('',#2493,#2497,#1209,.T.);
#3124=EDGE_CURVE('',#2499,#2500,#1553,.T.);
#3125=EDGE_CURVE('',#2500,#2498,#1210,.T.);
#3126=EDGE_CURVE('',#2497,#2499,#1211,.T.);
#3127=EDGE_CURVE('',#2501,#2502,#1554,.T.);
#3128=EDGE_CURVE('',#2502,#2500,#1212,.T.);
#3129=EDGE_CURVE('',#2499,#2501,#1213,.T.);
#3130=EDGE_CURVE('',#2503,#2504,#1555,.T.);
#3131=EDGE_CURVE('',#2504,#2502,#1214,.T.);
#3132=EDGE_CURVE('',#2501,#2503,#1215,.T.);
#3133=EDGE_CURVE('',#2505,#2506,#1556,.T.);
#3134=EDGE_CURVE('',#2506,#2504,#1216,.T.);
#3135=EDGE_CURVE('',#2503,#2505,#1217,.T.);
#3136=EDGE_CURVE('',#2507,#2508,#1557,.T.);
#3137=EDGE_CURVE('',#2508,#2506,#1218,.T.);
#3138=EDGE_CURVE('',#2505,#2507,#1219,.T.);
#3139=EDGE_CURVE('',#2509,#2510,#1558,.T.);
#3140=EDGE_CURVE('',#2510,#2508,#1220,.T.);
#3141=EDGE_CURVE('',#2507,#2509,#1221,.T.);
#3142=EDGE_CURVE('',#2511,#2512,#1559,.T.);
#3143=EDGE_CURVE('',#2512,#2510,#1222,.T.);
#3144=EDGE_CURVE('',#2509,#2511,#1223,.T.);
#3145=EDGE_CURVE('',#2513,#2514,#1560,.T.);
#3146=EDGE_CURVE('',#2514,#2512,#1224,.T.);
#3147=EDGE_CURVE('',#2511,#2513,#1225,.T.);
#3148=EDGE_CURVE('',#2515,#2516,#1561,.T.);
#3149=EDGE_CURVE('',#2515,#2517,#1226,.T.);
#3150=EDGE_CURVE('',#2518,#2517,#1072,.T.);
#3151=EDGE_CURVE('',#2518,#2519,#1073,.F.);
#3152=EDGE_CURVE('',#2519,#2516,#1227,.T.);
#3153=EDGE_CURVE('',#2520,#2521,#1562,.T.);
#3154=EDGE_CURVE('',#2521,#2522,#1228,.T.);
#3155=EDGE_CURVE('',#2523,#2522,#1074,.F.);
#3156=EDGE_CURVE('',#2523,#2520,#1229,.T.);
#3157=EDGE_CURVE('',#2524,#2525,#1563,.T.);
#3158=EDGE_CURVE('',#2525,#2521,#1230,.T.);
#3159=EDGE_CURVE('',#2520,#2524,#1231,.T.);
#3160=EDGE_CURVE('',#2526,#2527,#1564,.T.);
#3161=EDGE_CURVE('',#2527,#2525,#1232,.T.);
#3162=EDGE_CURVE('',#2524,#2526,#1233,.T.);
#3163=EDGE_CURVE('',#2528,#2529,#1565,.T.);
#3164=EDGE_CURVE('',#2529,#2527,#1234,.T.);
#3165=EDGE_CURVE('',#2526,#2528,#1235,.T.);
#3166=EDGE_CURVE('',#2530,#2531,#1566,.T.);
#3167=EDGE_CURVE('',#2531,#2529,#1236,.T.);
#3168=EDGE_CURVE('',#2528,#2530,#1237,.T.);
#3169=EDGE_CURVE('',#2532,#2533,#1567,.T.);
#3170=EDGE_CURVE('',#2533,#2531,#1238,.T.);
#3171=EDGE_CURVE('',#2530,#2532,#1239,.T.);
#3172=EDGE_CURVE('',#2534,#2535,#1568,.T.);
#3173=EDGE_CURVE('',#2535,#2533,#1240,.T.);
#3174=EDGE_CURVE('',#2532,#2534,#1241,.T.);
#3175=EDGE_CURVE('',#2536,#2537,#1569,.T.);
#3176=EDGE_CURVE('',#2537,#2535,#1242,.T.);
#3177=EDGE_CURVE('',#2534,#2536,#1243,.T.);
#3178=EDGE_CURVE('',#2538,#2539,#1570,.T.);
#3179=EDGE_CURVE('',#2539,#2537,#1244,.T.);
#3180=EDGE_CURVE('',#2536,#2538,#1245,.T.);
#3181=EDGE_CURVE('',#2540,#2541,#1571,.T.);
#3182=EDGE_CURVE('',#2541,#2539,#1246,.T.);
#3183=EDGE_CURVE('',#2538,#2540,#1247,.T.);
#3184=EDGE_CURVE('',#2542,#2543,#1572,.T.);
#3185=EDGE_CURVE('',#2542,#2544,#1248,.T.);
#3186=EDGE_CURVE('',#2544,#2545,#1075,.F.);
#3187=EDGE_CURVE('',#2546,#2545,#1076,.T.);
#3188=EDGE_CURVE('',#2546,#2543,#1249,.T.);
#3189=EDGE_CURVE('',#2547,#2548,#1573,.T.);
#3190=EDGE_CURVE('',#2548,#2549,#1250,.T.);
#3191=EDGE_CURVE('',#2550,#2549,#1077,.T.);
#3192=EDGE_CURVE('',#2547,#2550,#1251,.T.);
#3193=EDGE_CURVE('',#2551,#2552,#1574,.T.);
#3194=EDGE_CURVE('',#2552,#2548,#1252,.T.);
#3195=EDGE_CURVE('',#2551,#2547,#1253,.T.);
#3196=EDGE_CURVE('',#2553,#2554,#1575,.T.);
#3197=EDGE_CURVE('',#2554,#2552,#1254,.T.);
#3198=EDGE_CURVE('',#2553,#2551,#1255,.T.);
#3199=EDGE_CURVE('',#2555,#2556,#1576,.T.);
#3200=EDGE_CURVE('',#2556,#2554,#1256,.T.);
#3201=EDGE_CURVE('',#2555,#2553,#1257,.T.);
#3202=EDGE_CURVE('',#2557,#2558,#1577,.T.);
#3203=EDGE_CURVE('',#2558,#2556,#1258,.T.);
#3204=EDGE_CURVE('',#2557,#2555,#1259,.T.);
#3205=EDGE_CURVE('',#2559,#2560,#1578,.T.);
#3206=EDGE_CURVE('',#2560,#2558,#1260,.T.);
#3207=EDGE_CURVE('',#2559,#2557,#1261,.T.);
#3208=EDGE_CURVE('',#2561,#2562,#1579,.T.);
#3209=EDGE_CURVE('',#2562,#2560,#1262,.T.);
#3210=EDGE_CURVE('',#2561,#2559,#1263,.T.);
#3211=EDGE_CURVE('',#2563,#2564,#1580,.T.);
#3212=EDGE_CURVE('',#2564,#2562,#1264,.T.);
#3213=EDGE_CURVE('',#2563,#2561,#1265,.T.);
#3214=EDGE_CURVE('',#2565,#2566,#1581,.T.);
#3215=EDGE_CURVE('',#2566,#2564,#1266,.T.);
#3216=EDGE_CURVE('',#2565,#2563,#1267,.T.);
#3217=EDGE_CURVE('',#2567,#2568,#1582,.T.);
#3218=EDGE_CURVE('',#2568,#2566,#1268,.T.);
#3219=EDGE_CURVE('',#2567,#2565,#1269,.T.);
#3220=EDGE_CURVE('',#2569,#2570,#1583,.T.);
#3221=EDGE_CURVE('',#2570,#2568,#1270,.T.);
#3222=EDGE_CURVE('',#2569,#2567,#1271,.T.);
#3223=EDGE_CURVE('',#2571,#2572,#1584,.T.);
#3224=EDGE_CURVE('',#2573,#2571,#1272,.T.);
#3225=EDGE_CURVE('',#2574,#2573,#1078,.T.);
#3226=EDGE_CURVE('',#2574,#2572,#1273,.T.);
#3227=EDGE_CURVE('',#2575,#2576,#1585,.T.);
#3228=EDGE_CURVE('',#2576,#2577,#1274,.T.);
#3229=EDGE_CURVE('',#2578,#2577,#1079,.T.);
#3230=EDGE_CURVE('',#2575,#2578,#1275,.T.);
#3231=EDGE_CURVE('',#2579,#2580,#1586,.T.);
#3232=EDGE_CURVE('',#2580,#2576,#1276,.T.);
#3233=EDGE_CURVE('',#2579,#2575,#1277,.T.);
#3234=EDGE_CURVE('',#2581,#2582,#1587,.T.);
#3235=EDGE_CURVE('',#2582,#2580,#1278,.T.);
#3236=EDGE_CURVE('',#2581,#2579,#1279,.T.);
#3237=EDGE_CURVE('',#2583,#2584,#1588,.T.);
#3238=EDGE_CURVE('',#2584,#2582,#1280,.T.);
#3239=EDGE_CURVE('',#2583,#2581,#1281,.T.);
#3240=EDGE_CURVE('',#2585,#2586,#1589,.T.);
#3241=EDGE_CURVE('',#2586,#2584,#1282,.T.);
#3242=EDGE_CURVE('',#2585,#2583,#1283,.T.);
#3243=EDGE_CURVE('',#2587,#2588,#1590,.T.);
#3244=EDGE_CURVE('',#2588,#2586,#1284,.T.);
#3245=EDGE_CURVE('',#2587,#2585,#1285,.T.);
#3246=EDGE_CURVE('',#2589,#2590,#1591,.T.);
#3247=EDGE_CURVE('',#2590,#2588,#1286,.T.);
#3248=EDGE_CURVE('',#2589,#2587,#1287,.T.);
#3249=EDGE_CURVE('',#2591,#2592,#1592,.T.);
#3250=EDGE_CURVE('',#2592,#2590,#1288,.T.);
#3251=EDGE_CURVE('',#2591,#2589,#1289,.T.);
#3252=EDGE_CURVE('',#2593,#2594,#1593,.T.);
#3253=EDGE_CURVE('',#2594,#2592,#1290,.T.);
#3254=EDGE_CURVE('',#2593,#2591,#1291,.T.);
#3255=EDGE_CURVE('',#2595,#2596,#1594,.T.);
#3256=EDGE_CURVE('',#2596,#2594,#1292,.T.);
#3257=EDGE_CURVE('',#2595,#2593,#1293,.T.);
#3258=EDGE_CURVE('',#2597,#2598,#1595,.T.);
#3259=EDGE_CURVE('',#2598,#2596,#1294,.T.);
#3260=EDGE_CURVE('',#2597,#2595,#1295,.T.);
#3261=EDGE_CURVE('',#2599,#2600,#1596,.T.);
#3262=EDGE_CURVE('',#2601,#2599,#1296,.T.);
#3263=EDGE_CURVE('',#2602,#2601,#1080,.T.);
#3264=EDGE_CURVE('',#2602,#2600,#1297,.T.);
#3265=EDGE_CURVE('',#2603,#2604,#1597,.T.);
#3266=EDGE_CURVE('',#2604,#2605,#1298,.T.);
#3267=EDGE_CURVE('',#2606,#2605,#1081,.T.);
#3268=EDGE_CURVE('',#2603,#2606,#1299,.T.);
#3269=EDGE_CURVE('',#2607,#2608,#1598,.T.);
#3270=EDGE_CURVE('',#2608,#2604,#1300,.T.);
#3271=EDGE_CURVE('',#2607,#2603,#1301,.T.);
#3272=EDGE_CURVE('',#2609,#2610,#1599,.T.);
#3273=EDGE_CURVE('',#2610,#2608,#1302,.T.);
#3274=EDGE_CURVE('',#2609,#2607,#1303,.T.);
#3275=EDGE_CURVE('',#2611,#2612,#1600,.T.);
#3276=EDGE_CURVE('',#2612,#2610,#1304,.T.);
#3277=EDGE_CURVE('',#2611,#2609,#1305,.T.);
#3278=EDGE_CURVE('',#2613,#2614,#1601,.T.);
#3279=EDGE_CURVE('',#2614,#2612,#1306,.T.);
#3280=EDGE_CURVE('',#2613,#2611,#1307,.T.);
#3281=EDGE_CURVE('',#2615,#2616,#1602,.T.);
#3282=EDGE_CURVE('',#2616,#2614,#1308,.T.);
#3283=EDGE_CURVE('',#2615,#2613,#1309,.T.);
#3284=EDGE_CURVE('',#2617,#2618,#1603,.T.);
#3285=EDGE_CURVE('',#2618,#2616,#1310,.T.);
#3286=EDGE_CURVE('',#2617,#2615,#1311,.T.);
#3287=EDGE_CURVE('',#2619,#2620,#1604,.T.);
#3288=EDGE_CURVE('',#2620,#2618,#1312,.T.);
#3289=EDGE_CURVE('',#2619,#2617,#1313,.T.);
#3290=EDGE_CURVE('',#2621,#2622,#1605,.T.);
#3291=EDGE_CURVE('',#2622,#2620,#1314,.T.);
#3292=EDGE_CURVE('',#2621,#2619,#1315,.T.);
#3293=EDGE_CURVE('',#2623,#2624,#1606,.T.);
#3294=EDGE_CURVE('',#2624,#2622,#1316,.T.);
#3295=EDGE_CURVE('',#2623,#2621,#1317,.T.);
#3296=EDGE_CURVE('',#2625,#2626,#1607,.T.);
#3297=EDGE_CURVE('',#2626,#2624,#1318,.T.);
#3298=EDGE_CURVE('',#2625,#2623,#1319,.T.);
#3299=EDGE_CURVE('',#2627,#2628,#1608,.T.);
#3300=EDGE_CURVE('',#2629,#2627,#1320,.T.);
#3301=EDGE_CURVE('',#2630,#2629,#1082,.T.);
#3302=EDGE_CURVE('',#2630,#2628,#1321,.T.);
#3303=EDGE_CURVE('',#2631,#2632,#1609,.T.);
#3304=EDGE_CURVE('',#2632,#2633,#1322,.T.);
#3305=EDGE_CURVE('',#2634,#2633,#1083,.T.);
#3306=EDGE_CURVE('',#2631,#2634,#1323,.T.);
#3307=EDGE_CURVE('',#2635,#2636,#1610,.T.);
#3308=EDGE_CURVE('',#2636,#2632,#1324,.T.);
#3309=EDGE_CURVE('',#2635,#2631,#1325,.T.);
#3310=EDGE_CURVE('',#2637,#2638,#1611,.T.);
#3311=EDGE_CURVE('',#2638,#2636,#1326,.T.);
#3312=EDGE_CURVE('',#2637,#2635,#1327,.T.);
#3313=EDGE_CURVE('',#2639,#2640,#1612,.T.);
#3314=EDGE_CURVE('',#2640,#2638,#1328,.T.);
#3315=EDGE_CURVE('',#2639,#2637,#1329,.T.);
#3316=EDGE_CURVE('',#2641,#2642,#1613,.T.);
#3317=EDGE_CURVE('',#2642,#2640,#1330,.T.);
#3318=EDGE_CURVE('',#2641,#2639,#1331,.T.);
#3319=EDGE_CURVE('',#2643,#2644,#1614,.T.);
#3320=EDGE_CURVE('',#2644,#2642,#1332,.T.);
#3321=EDGE_CURVE('',#2643,#2641,#1333,.T.);
#3322=EDGE_CURVE('',#2645,#2646,#1615,.T.);
#3323=EDGE_CURVE('',#2646,#2644,#1334,.T.);
#3324=EDGE_CURVE('',#2645,#2643,#1335,.T.);
#3325=EDGE_CURVE('',#2647,#2648,#1616,.T.);
#3326=EDGE_CURVE('',#2648,#2646,#1336,.T.);
#3327=EDGE_CURVE('',#2647,#2645,#1337,.T.);
#3328=EDGE_CURVE('',#2649,#2650,#1617,.T.);
#3329=EDGE_CURVE('',#2650,#2648,#1338,.T.);
#3330=EDGE_CURVE('',#2649,#2647,#1339,.T.);
#3331=EDGE_CURVE('',#2651,#2652,#1618,.T.);
#3332=EDGE_CURVE('',#2652,#2650,#1340,.T.);
#3333=EDGE_CURVE('',#2651,#2649,#1341,.T.);
#3334=EDGE_CURVE('',#2653,#2654,#1619,.T.);
#3335=EDGE_CURVE('',#2654,#2652,#1342,.T.);
#3336=EDGE_CURVE('',#2653,#2651,#1343,.T.);
#3337=EDGE_CURVE('',#2655,#2656,#1620,.T.);
#3338=EDGE_CURVE('',#2657,#2655,#1344,.T.);
#3339=EDGE_CURVE('',#2658,#2657,#1084,.T.);
#3340=EDGE_CURVE('',#2658,#2656,#1345,.T.);
#3341=EDGE_CURVE('',#2659,#2660,#1621,.T.);
#3342=EDGE_CURVE('',#2660,#2661,#313,.T.);
#3343=EDGE_CURVE('',#2661,#2662,#1622,.T.);
#3344=EDGE_CURVE('',#2659,#2662,#314,.T.);
#3345=EDGE_CURVE('',#2660,#2663,#1623,.T.);
#3346=EDGE_CURVE('',#2663,#2664,#315,.T.);
#3347=EDGE_CURVE('',#2664,#2661,#1624,.T.);
#3348=EDGE_CURVE('',#2663,#2665,#1625,.T.);
#3349=EDGE_CURVE('',#2665,#2666,#316,.T.);
#3350=EDGE_CURVE('',#2666,#2664,#1626,.T.);
#3351=EDGE_CURVE('',#2665,#2667,#1627,.T.);
#3352=EDGE_CURVE('',#2667,#2668,#317,.T.);
#3353=EDGE_CURVE('',#2668,#2666,#1628,.T.);
#3354=EDGE_CURVE('',#2669,#2668,#1629,.T.);
#3355=EDGE_CURVE('',#2667,#2670,#1630,.T.);
#3356=EDGE_CURVE('',#2670,#2669,#318,.T.);
#3357=EDGE_CURVE('',#2662,#2669,#1631,.T.);
#3358=EDGE_CURVE('',#2670,#2659,#1632,.T.);
#3359=EDGE_CURVE('',#2671,#2669,#1633,.T.);
#3360=EDGE_CURVE('',#2672,#2671,#1634,.T.);
#3361=EDGE_CURVE('',#2673,#2672,#1635,.T.);
#3362=EDGE_CURVE('',#2674,#2673,#1636,.T.);
#3363=EDGE_CURVE('',#2674,#2668,#1637,.T.);
#3364=EDGE_CURVE('',#2675,#2662,#1638,.T.);
#3365=EDGE_CURVE('',#2545,#2675,#1639,.T.);
#3366=EDGE_CURVE('',#2671,#2545,#1640,.T.);
#3367=EDGE_CURVE('',#2676,#2661,#1641,.T.);
#3368=EDGE_CURVE('',#2675,#2676,#1642,.T.);
#3369=EDGE_CURVE('',#2677,#2678,#1643,.T.);
#3370=EDGE_CURVE('',#2679,#2677,#1085,.T.);
#3371=EDGE_CURVE('',#2680,#2679,#1644,.T.);
#3372=EDGE_CURVE('',#2681,#2680,#1645,.T.);
#3373=EDGE_CURVE('',#2682,#2681,#1646,.T.);
#3374=EDGE_CURVE('',#2683,#2682,#1086,.T.);
#3375=EDGE_CURVE('',#2684,#2683,#1087,.T.);
#3376=EDGE_CURVE('',#2685,#2684,#1647,.T.);
#3377=EDGE_CURVE('',#2678,#2685,#1648,.T.);
#3378=EDGE_CURVE('',#2679,#2686,#1346,.T.);
#3379=EDGE_CURVE('',#2686,#2677,#1347,.T.);
#3380=EDGE_CURVE('',#2678,#2687,#319,.T.);
#3381=EDGE_CURVE('',#2687,#2688,#1649,.T.);
#3382=EDGE_CURVE('',#2680,#2688,#320,.T.);
#3383=EDGE_CURVE('',#2685,#2689,#321,.T.);
#3384=EDGE_CURVE('',#2689,#2687,#1650,.T.);
#3385=EDGE_CURVE('',#2684,#2682,#1348,.T.);
#3386=EDGE_CURVE('',#2681,#2690,#322,.T.);
#3387=EDGE_CURVE('',#2690,#2689,#1651,.T.);
#3388=EDGE_CURVE('',#2688,#2690,#1652,.T.);
#3389=EDGE_CURVE('',#2691,#2688,#1653,.T.);
#3390=EDGE_CURVE('',#2691,#2692,#1654,.T.);
#3391=EDGE_CURVE('',#2692,#2690,#1655,.T.);
#3392=EDGE_CURVE('',#2693,#2687,#1656,.T.);
#3393=EDGE_CURVE('',#2693,#2691,#1657,.T.);
#3394=EDGE_CURVE('',#2686,#2694,#1088,.T.);
#3395=EDGE_CURVE('',#2694,#2695,#1089,.T.);
#3396=EDGE_CURVE('',#2695,#2694,#1090,.T.);
#3397=EDGE_CURVE('',#2683,#2696,#1091,.T.);
#3398=EDGE_CURVE('',#2696,#2697,#1092,.T.);
#3399=EDGE_CURVE('',#2697,#2696,#1093,.T.);
#3400=EDGE_CURVE('',#2695,#2698,#1658,.T.);
#3401=EDGE_CURVE('',#2698,#2698,#1094,.T.);
#3402=EDGE_CURVE('',#2697,#2699,#1659,.T.);
#3403=EDGE_CURVE('',#2699,#2699,#1095,.T.);
#3404=EDGE_CURVE('',#2656,#2654,#1349,.T.);
#3405=EDGE_CURVE('',#2655,#2653,#1350,.T.);
#3406=EDGE_CURVE('',#2633,#2496,#1351,.T.);
#3407=EDGE_CURVE('',#2673,#2658,#1352,.T.);
#3408=EDGE_CURVE('',#2517,#2673,#1353,.T.);
#3409=EDGE_CURVE('',#2513,#2515,#1354,.T.);
#3410=EDGE_CURVE('',#2495,#2634,#1355,.T.);
#3411=EDGE_CURVE('',#2516,#2514,#1356,.T.);
#3412=EDGE_CURVE('',#2657,#2519,#1357,.T.);
#3413=EDGE_CURVE('',#2700,#2701,#1660,.T.);
#3414=EDGE_CURVE('',#2702,#2700,#1661,.T.);
#3415=EDGE_CURVE('',#2703,#2702,#1662,.T.);
#3416=EDGE_CURVE('',#2704,#2703,#1663,.T.);
#3417=EDGE_CURVE('',#2705,#2704,#1664,.T.);
#3418=EDGE_CURVE('',#2701,#2705,#1665,.T.);
#3419=EDGE_CURVE('',#2706,#2707,#1666,.T.);
#3420=EDGE_CURVE('',#2707,#2708,#1667,.T.);
#3421=EDGE_CURVE('',#2708,#2709,#1668,.T.);
#3422=EDGE_CURVE('',#2709,#2706,#1669,.T.);
#3423=EDGE_CURVE('',#2710,#2711,#1670,.T.);
#3424=EDGE_CURVE('',#2711,#2712,#1671,.T.);
#3425=EDGE_CURVE('',#2712,#2713,#1672,.T.);
#3426=EDGE_CURVE('',#2713,#2710,#1673,.T.);
#3427=EDGE_CURVE('',#2714,#2715,#1674,.T.);
#3428=EDGE_CURVE('',#2715,#2716,#1675,.T.);
#3429=EDGE_CURVE('',#2716,#2717,#1676,.T.);
#3430=EDGE_CURVE('',#2717,#2714,#1677,.T.);
#3431=EDGE_CURVE('',#2549,#2523,#1358,.T.);
#3432=EDGE_CURVE('',#2522,#2550,#1359,.T.);
#3433=EDGE_CURVE('',#2577,#2470,#1360,.T.);
#3434=EDGE_CURVE('',#2469,#2578,#1361,.T.);
#3435=EDGE_CURVE('',#2605,#2444,#1362,.T.);
#3436=EDGE_CURVE('',#2443,#2606,#1363,.T.);
#3437=EDGE_CURVE('',#2628,#2626,#1364,.T.);
#3438=EDGE_CURVE('',#2627,#2625,#1365,.T.);
#3439=EDGE_CURVE('',#2465,#2630,#1366,.T.);
#3440=EDGE_CURVE('',#2461,#2463,#1367,.T.);
#3441=EDGE_CURVE('',#2464,#2462,#1368,.T.);
#3442=EDGE_CURVE('',#2629,#2466,#1369,.T.);
#3443=EDGE_CURVE('',#2600,#2598,#1370,.T.);
#3444=EDGE_CURVE('',#2599,#2597,#1371,.T.);
#3445=EDGE_CURVE('',#2491,#2602,#1372,.T.);
#3446=EDGE_CURVE('',#2487,#2489,#1373,.T.);
#3447=EDGE_CURVE('',#2490,#2488,#1374,.T.);
#3448=EDGE_CURVE('',#2601,#2492,#1375,.T.);
#3449=EDGE_CURVE('',#2572,#2570,#1376,.T.);
#3450=EDGE_CURVE('',#2571,#2569,#1377,.T.);
#3451=EDGE_CURVE('',#2544,#2574,#1378,.T.);
#3452=EDGE_CURVE('',#2540,#2542,#1379,.T.);
#3453=EDGE_CURVE('',#2543,#2541,#1380,.T.);
#3454=EDGE_CURVE('',#2672,#2546,#1381,.T.);
#3455=EDGE_CURVE('',#2573,#2672,#1382,.T.);
#3456=EDGE_CURVE('',#2676,#2718,#1678,.T.);
#3457=EDGE_CURVE('',#2718,#2719,#1679,.T.);
#3458=EDGE_CURVE('',#2719,#2518,#1680,.T.);
#3459=EDGE_CURVE('',#2720,#2721,#1681,.T.);
#3460=EDGE_CURVE('',#2721,#2722,#1682,.T.);
#3461=EDGE_CURVE('',#2722,#2723,#1683,.T.);
#3462=EDGE_CURVE('',#2723,#2720,#1684,.T.);
#3463=EDGE_CURVE('',#2724,#2725,#1685,.T.);
#3464=EDGE_CURVE('',#2725,#2726,#1686,.T.);
#3465=EDGE_CURVE('',#2726,#2727,#1687,.T.);
#3466=EDGE_CURVE('',#2727,#2724,#1688,.T.);
#3467=EDGE_CURVE('',#2728,#2729,#1689,.T.);
#3468=EDGE_CURVE('',#2729,#2730,#1690,.T.);
#3469=EDGE_CURVE('',#2730,#2731,#1691,.T.);
#3470=EDGE_CURVE('',#2731,#2728,#1692,.T.);
#3471=EDGE_CURVE('',#2518,#2674,#1693,.T.);
#3472=EDGE_CURVE('',#2728,#2707,#1694,.T.);
#3473=EDGE_CURVE('',#2729,#2706,#1695,.T.);
#3474=EDGE_CURVE('',#2731,#2708,#1696,.T.);
#3475=EDGE_CURVE('',#2730,#2709,#1697,.T.);
#3476=EDGE_CURVE('',#2724,#2711,#1698,.T.);
#3477=EDGE_CURVE('',#2725,#2710,#1699,.T.);
#3478=EDGE_CURVE('',#2727,#2712,#1700,.T.);
#3479=EDGE_CURVE('',#2726,#2713,#1701,.T.);
#3480=EDGE_CURVE('',#2720,#2715,#1702,.T.);
#3481=EDGE_CURVE('',#2721,#2714,#1703,.T.);
#3482=EDGE_CURVE('',#2723,#2716,#1704,.T.);
#3483=EDGE_CURVE('',#2722,#2717,#1705,.T.);
#3484=EDGE_CURVE('',#2692,#2732,#1706,.T.);
#3485=EDGE_CURVE('',#2732,#2693,#1707,.T.);
#3486=EDGE_CURVE('',#2733,#2734,#1708,.T.);
#3487=EDGE_CURVE('',#2735,#2733,#1709,.T.);
#3488=EDGE_CURVE('',#2736,#2735,#1710,.T.);
#3489=EDGE_CURVE('',#2737,#2736,#1711,.T.);
#3490=EDGE_CURVE('',#2738,#2737,#1712,.T.);
#3491=EDGE_CURVE('',#2734,#2738,#1713,.T.);
#3492=EDGE_CURVE('',#2732,#2689,#1714,.T.);
#3493=EDGE_CURVE('',#2718,#2664,#1715,.T.);
#3494=EDGE_CURVE('',#2719,#2666,#1716,.T.);
#3495=EDGE_CURVE('',#2705,#2736,#1717,.T.);
#3496=EDGE_CURVE('',#2704,#2737,#1718,.T.);
#3497=EDGE_CURVE('',#2701,#2735,#1719,.T.);
#3498=EDGE_CURVE('',#2700,#2733,#1720,.T.);
#3499=EDGE_CURVE('',#2702,#2734,#1721,.T.);
#3500=EDGE_CURVE('',#2703,#2738,#1722,.T.);
#3501=EDGE_CURVE('',#2739,#2740,#1096,.F.);
#3502=EDGE_CURVE('',#2741,#2739,#1097,.F.);
#3503=EDGE_CURVE('',#2740,#2741,#1098,.F.);
#3504=EDGE_CURVE('',#2742,#2743,#1099,.F.);
#3505=EDGE_CURVE('',#2744,#2742,#1100,.F.);
#3506=EDGE_CURVE('',#2743,#2744,#1101,.F.);
#3507=EDGE_CURVE('',#2745,#2746,#1102,.F.);
#3508=EDGE_CURVE('',#2747,#2745,#1103,.F.);
#3509=EDGE_CURVE('',#2746,#2747,#1104,.F.);
#3510=EDGE_CURVE('',#2748,#2749,#1105,.F.);
#3511=EDGE_CURVE('',#2750,#2748,#1106,.F.);
#3512=EDGE_CURVE('',#2749,#2750,#1107,.F.);
#3513=EDGE_CURVE('',#2751,#2752,#1108,.F.);
#3514=EDGE_CURVE('',#2753,#2751,#1109,.F.);
#3515=EDGE_CURVE('',#2752,#2753,#1110,.F.);
#3516=EDGE_CURVE('',#2754,#2755,#1111,.F.);
#3517=EDGE_CURVE('',#2756,#2754,#1112,.F.);
#3518=EDGE_CURVE('',#2755,#2756,#1113,.F.);
#3519=EDGE_CURVE('',#2757,#2758,#1114,.F.);
#3520=EDGE_CURVE('',#2759,#2757,#1115,.F.);
#3521=EDGE_CURVE('',#2758,#2759,#1116,.F.);
#3522=EDGE_CURVE('',#2760,#2761,#1117,.F.);
#3523=EDGE_CURVE('',#2762,#2760,#1118,.F.);
#3524=EDGE_CURVE('',#2761,#2762,#1119,.F.);
#3525=EDGE_CURVE('',#2760,#2753,#1723,.T.);
#3526=EDGE_CURVE('',#2751,#2762,#1724,.T.);
#3527=EDGE_CURVE('',#2757,#2761,#1725,.T.);
#3528=EDGE_CURVE('',#2762,#2759,#1726,.T.);
#3529=EDGE_CURVE('',#2754,#2760,#1727,.T.);
#3530=EDGE_CURVE('',#2761,#2756,#1728,.T.);
#3531=EDGE_CURVE('',#2745,#2758,#1729,.T.);
#3532=EDGE_CURVE('',#2759,#2747,#1730,.T.);
#3533=EDGE_CURVE('',#2748,#2757,#1731,.T.);
#3534=EDGE_CURVE('',#2758,#2750,#1732,.T.);
#3535=EDGE_CURVE('',#2749,#2755,#1733,.T.);
#3536=EDGE_CURVE('',#2756,#2748,#1734,.T.);
#3537=EDGE_CURVE('',#2755,#2743,#1735,.T.);
#3538=EDGE_CURVE('',#2744,#2754,#1736,.T.);
#3539=EDGE_CURVE('',#2742,#2752,#1737,.T.);
#3540=EDGE_CURVE('',#2753,#2744,#1738,.T.);
#3541=EDGE_CURVE('',#2752,#2746,#1739,.T.);
#3542=EDGE_CURVE('',#2747,#2751,#1740,.T.);
#3543=EDGE_CURVE('',#2740,#2749,#1741,.T.);
#3544=EDGE_CURVE('',#2750,#2739,#1742,.T.);
#3545=EDGE_CURVE('',#2739,#2745,#1743,.T.);
#3546=EDGE_CURVE('',#2746,#2741,#1744,.T.);
#3547=EDGE_CURVE('',#2743,#2740,#1745,.T.);
#3548=EDGE_CURVE('',#2741,#2742,#1746,.T.);
#3549=EDGE_CURVE('',#2763,#2764,#1747,.T.);
#3550=EDGE_CURVE('',#2764,#2765,#1748,.T.);
#3551=EDGE_CURVE('',#2765,#2766,#1749,.T.);
#3552=EDGE_CURVE('',#2766,#2763,#1750,.T.);
#3553=EDGE_CURVE('',#2767,#2767,#1120,.T.);
#3554=EDGE_CURVE('',#2768,#2768,#1121,.T.);
#3555=EDGE_CURVE('',#2769,#2770,#1751,.T.);
#3556=EDGE_CURVE('',#2770,#2771,#1752,.T.);
#3557=EDGE_CURVE('',#2771,#2772,#1753,.T.);
#3558=EDGE_CURVE('',#2772,#2769,#1754,.T.);
#3559=EDGE_CURVE('',#2773,#2773,#1122,.T.);
#3560=EDGE_CURVE('',#2774,#2774,#1123,.T.);
#3561=EDGE_CURVE('',#2774,#2768,#1755,.T.);
#3562=EDGE_CURVE('',#2773,#2767,#1756,.T.);
#3563=EDGE_CURVE('',#2769,#2764,#1757,.T.);
#3564=EDGE_CURVE('',#2770,#2763,#1758,.T.);
#3565=EDGE_CURVE('',#2772,#2765,#1759,.T.);
#3566=EDGE_CURVE('',#2771,#2766,#1760,.T.);
#3567=EDGE_CURVE('',#2775,#2775,#1124,.T.);
#3568=EDGE_CURVE('',#2775,#2776,#1761,.T.);
#3569=EDGE_CURVE('',#2776,#2776,#1125,.T.);
#3570=EDGE_CURVE('',#2777,#2777,#1126,.T.);
#3571=EDGE_CURVE('',#2777,#2778,#1762,.T.);
#3572=EDGE_CURVE('',#2778,#2778,#1127,.T.);
#3573=EDGE_CURVE('',#2779,#2780,#1763,.T.);
#3574=EDGE_CURVE('',#2780,#2781,#1764,.T.);
#3575=EDGE_CURVE('',#2782,#2781,#1765,.T.);
#3576=EDGE_CURVE('',#2779,#2782,#1766,.T.);
#3577=EDGE_CURVE('',#2783,#2779,#1767,.T.);
#3578=EDGE_CURVE('',#2784,#2782,#1768,.T.);
#3579=EDGE_CURVE('',#2783,#2784,#1769,.T.);
#3580=EDGE_CURVE('',#2785,#2783,#1770,.T.);
#3581=EDGE_CURVE('',#2786,#2784,#1771,.T.);
#3582=EDGE_CURVE('',#2785,#2786,#1772,.T.);
#3583=EDGE_CURVE('',#2780,#2785,#1773,.T.);
#3584=EDGE_CURVE('',#2781,#2786,#1774,.T.);
#3585=EDGE_CURVE('',#2787,#2788,#1775,.T.);
#3586=EDGE_CURVE('',#2788,#2789,#1776,.T.);
#3587=EDGE_CURVE('',#2790,#2789,#1777,.T.);
#3588=EDGE_CURVE('',#2787,#2790,#1778,.T.);
#3589=EDGE_CURVE('',#2791,#2787,#1779,.T.);
#3590=EDGE_CURVE('',#2792,#2790,#1780,.T.);
#3591=EDGE_CURVE('',#2791,#2792,#1781,.T.);
#3592=EDGE_CURVE('',#2793,#2791,#1782,.T.);
#3593=EDGE_CURVE('',#2794,#2792,#1783,.T.);
#3594=EDGE_CURVE('',#2793,#2794,#1784,.T.);
#3595=EDGE_CURVE('',#2788,#2793,#1785,.T.);
#3596=EDGE_CURVE('',#2789,#2794,#1786,.T.);
#3597=EDGE_CURVE('',#2795,#2795,#1128,.T.);
#3598=EDGE_CURVE('',#2795,#2796,#1787,.T.);
#3599=EDGE_CURVE('',#2796,#2796,#1129,.T.);
#3600=EDGE_CURVE('',#2797,#2797,#1130,.T.);
#3601=EDGE_CURVE('',#2797,#2798,#1788,.T.);
#3602=EDGE_CURVE('',#2798,#2798,#1131,.T.);
#3603=EDGE_CURVE('',#2799,#2799,#1132,.T.);
#3604=EDGE_CURVE('',#2799,#2800,#1789,.T.);
#3605=EDGE_CURVE('',#2800,#2800,#1133,.T.);
#3606=EDGE_CURVE('',#2801,#2801,#1134,.T.);
#3607=EDGE_CURVE('',#2801,#2802,#1790,.T.);
#3608=EDGE_CURVE('',#2802,#2802,#1135,.T.);
#3609=EDGE_CURVE('',#2803,#2804,#1791,.T.);
#3610=EDGE_CURVE('',#2803,#2805,#1792,.T.);
#3611=EDGE_CURVE('',#2806,#2805,#1793,.T.);
#3612=EDGE_CURVE('',#2804,#2806,#1794,.T.);
#3613=EDGE_CURVE('',#2807,#2803,#1795,.T.);
#3614=EDGE_CURVE('',#2807,#2808,#1796,.T.);
#3615=EDGE_CURVE('',#2805,#2808,#1797,.T.);
#3616=EDGE_CURVE('',#2809,#2807,#1798,.T.);
#3617=EDGE_CURVE('',#2809,#2810,#1799,.T.);
#3618=EDGE_CURVE('',#2808,#2810,#1800,.T.);
#3619=EDGE_CURVE('',#2804,#2809,#1801,.T.);
#3620=EDGE_CURVE('',#2810,#2806,#1802,.T.);
#3621=EDGE_CURVE('',#2811,#2812,#1803,.T.);
#3622=EDGE_CURVE('',#2811,#2813,#1804,.T.);
#3623=EDGE_CURVE('',#2814,#2813,#1805,.T.);
#3624=EDGE_CURVE('',#2812,#2814,#1806,.T.);
#3625=EDGE_CURVE('',#2815,#2811,#1807,.T.);
#3626=EDGE_CURVE('',#2815,#2816,#1808,.T.);
#3627=EDGE_CURVE('',#2813,#2816,#1809,.T.);
#3628=EDGE_CURVE('',#2817,#2815,#1810,.T.);
#3629=EDGE_CURVE('',#2817,#2818,#1811,.T.);
#3630=EDGE_CURVE('',#2816,#2818,#1812,.T.);
#3631=EDGE_CURVE('',#2812,#2817,#1813,.T.);
#3632=EDGE_CURVE('',#2818,#2814,#1814,.T.);
#3633=EDGE_CURVE('',#2819,#2820,#1815,.T.);
#3634=EDGE_CURVE('',#2819,#2821,#1816,.T.);
#3635=EDGE_CURVE('',#2822,#2821,#1817,.T.);
#3636=EDGE_CURVE('',#2820,#2822,#1818,.T.);
#3637=EDGE_CURVE('',#2823,#2819,#1819,.T.);
#3638=EDGE_CURVE('',#2823,#2824,#1820,.T.);
#3639=EDGE_CURVE('',#2821,#2824,#1821,.T.);
#3640=EDGE_CURVE('',#2825,#2823,#1822,.T.);
#3641=EDGE_CURVE('',#2825,#2826,#1823,.T.);
#3642=EDGE_CURVE('',#2824,#2826,#1824,.T.);
#3643=EDGE_CURVE('',#2820,#2825,#1825,.T.);
#3644=EDGE_CURVE('',#2826,#2822,#1826,.T.);
#3645=EDGE_CURVE('',#2827,#2828,#1827,.T.);
#3646=EDGE_CURVE('',#2828,#2829,#1828,.T.);
#3647=EDGE_CURVE('',#2830,#2829,#1829,.T.);
#3648=EDGE_CURVE('',#2827,#2830,#1830,.T.);
#3649=EDGE_CURVE('',#2831,#2827,#1831,.T.);
#3650=EDGE_CURVE('',#2832,#2830,#1832,.T.);
#3651=EDGE_CURVE('',#2831,#2832,#1833,.T.);
#3652=EDGE_CURVE('',#2833,#2831,#1834,.T.);
#3653=EDGE_CURVE('',#2834,#2832,#1835,.T.);
#3654=EDGE_CURVE('',#2833,#2834,#1836,.T.);
#3655=EDGE_CURVE('',#2828,#2833,#1837,.T.);
#3656=EDGE_CURVE('',#2829,#2834,#1838,.T.);
#3657=EDGE_CURVE('',#2835,#2835,#1136,.T.);
#3658=EDGE_CURVE('',#2835,#2836,#1839,.T.);
#3659=EDGE_CURVE('',#2836,#2836,#1137,.T.);
#3660=EDGE_CURVE('',#2837,#2838,#1840,.T.);
#3661=EDGE_CURVE('',#2838,#2839,#1841,.T.);
#3662=EDGE_CURVE('',#2840,#2839,#1842,.T.);
#3663=EDGE_CURVE('',#2837,#2840,#1843,.T.);
#3664=EDGE_CURVE('',#2841,#2837,#1844,.T.);
#3665=EDGE_CURVE('',#2842,#2840,#1845,.T.);
#3666=EDGE_CURVE('',#2841,#2842,#1846,.T.);
#3667=EDGE_CURVE('',#2843,#2841,#1847,.T.);
#3668=EDGE_CURVE('',#2844,#2842,#1848,.T.);
#3669=EDGE_CURVE('',#2843,#2844,#1849,.T.);
#3670=EDGE_CURVE('',#2838,#2843,#1850,.T.);
#3671=EDGE_CURVE('',#2839,#2844,#1851,.T.);
#3672=EDGE_CURVE('',#2845,#2845,#1138,.T.);
#3673=EDGE_CURVE('',#2845,#2846,#1852,.T.);
#3674=EDGE_CURVE('',#2846,#2846,#1139,.T.);
#3675=EDGE_CURVE('',#2847,#2848,#1853,.T.);
#3676=EDGE_CURVE('',#2848,#2849,#1854,.T.);
#3677=EDGE_CURVE('',#2850,#2849,#1855,.T.);
#3678=EDGE_CURVE('',#2847,#2850,#1856,.T.);
#3679=EDGE_CURVE('',#2851,#2847,#1857,.T.);
#3680=EDGE_CURVE('',#2852,#2850,#1858,.T.);
#3681=EDGE_CURVE('',#2851,#2852,#1859,.T.);
#3682=EDGE_CURVE('',#2853,#2851,#1860,.T.);
#3683=EDGE_CURVE('',#2854,#2852,#1861,.T.);
#3684=EDGE_CURVE('',#2853,#2854,#1862,.T.);
#3685=EDGE_CURVE('',#2848,#2853,#1863,.T.);
#3686=EDGE_CURVE('',#2849,#2854,#1864,.T.);
#3687=EDGE_CURVE('',#2855,#2856,#1865,.T.);
#3688=EDGE_CURVE('',#2855,#2857,#1383,.T.);
#3689=EDGE_CURVE('',#2857,#2858,#1140,.F.);
#3690=EDGE_CURVE('',#2858,#2856,#1384,.T.);
#3691=EDGE_CURVE('',#2859,#2860,#1866,.T.);
#3692=EDGE_CURVE('',#2859,#2855,#1385,.T.);
#3693=EDGE_CURVE('',#2856,#2860,#1386,.T.);
#3694=EDGE_CURVE('',#2861,#2862,#1867,.T.);
#3695=EDGE_CURVE('',#2861,#2859,#1387,.T.);
#3696=EDGE_CURVE('',#2860,#2862,#1388,.T.);
#3697=EDGE_CURVE('',#2863,#2864,#1868,.T.);
#3698=EDGE_CURVE('',#2863,#2861,#1389,.T.);
#3699=EDGE_CURVE('',#2862,#2864,#1390,.T.);
#3700=EDGE_CURVE('',#2865,#2866,#1869,.T.);
#3701=EDGE_CURVE('',#2865,#2863,#1391,.T.);
#3702=EDGE_CURVE('',#2864,#2866,#1392,.T.);
#3703=EDGE_CURVE('',#2867,#2868,#1870,.T.);
#3704=EDGE_CURVE('',#2867,#2865,#1393,.T.);
#3705=EDGE_CURVE('',#2866,#2868,#1394,.T.);
#3706=EDGE_CURVE('',#2869,#2870,#1871,.T.);
#3707=EDGE_CURVE('',#2869,#2867,#1395,.T.);
#3708=EDGE_CURVE('',#2868,#2870,#1396,.T.);
#3709=EDGE_CURVE('',#2871,#2872,#1872,.T.);
#3710=EDGE_CURVE('',#2871,#2869,#1397,.T.);
#3711=EDGE_CURVE('',#2870,#2872,#1398,.T.);
#3712=EDGE_CURVE('',#2873,#2874,#1873,.T.);
#3713=EDGE_CURVE('',#2873,#2871,#1399,.T.);
#3714=EDGE_CURVE('',#2872,#2874,#1400,.T.);
#3715=EDGE_CURVE('',#2875,#2876,#1874,.T.);
#3716=EDGE_CURVE('',#2875,#2873,#1401,.T.);
#3717=EDGE_CURVE('',#2874,#2876,#1402,.T.);
#3718=EDGE_CURVE('',#2877,#2878,#1875,.T.);
#3719=EDGE_CURVE('',#2877,#2879,#1403,.T.);
#3720=EDGE_CURVE('',#2879,#2880,#1141,.T.);
#3721=EDGE_CURVE('',#2878,#2880,#1404,.T.);
#3722=EDGE_CURVE('',#2881,#2882,#1876,.T.);
#3723=EDGE_CURVE('',#2881,#2877,#1405,.T.);
#3724=EDGE_CURVE('',#2882,#2878,#1406,.T.);
#3725=EDGE_CURVE('',#2883,#2884,#1877,.T.);
#3726=EDGE_CURVE('',#2883,#2881,#1407,.T.);
#3727=EDGE_CURVE('',#2884,#2882,#1408,.T.);
#3728=EDGE_CURVE('',#2885,#2886,#1878,.T.);
#3729=EDGE_CURVE('',#2885,#2883,#1409,.T.);
#3730=EDGE_CURVE('',#2886,#2884,#1410,.T.);
#3731=EDGE_CURVE('',#2887,#2888,#1879,.T.);
#3732=EDGE_CURVE('',#2887,#2885,#1411,.T.);
#3733=EDGE_CURVE('',#2888,#2886,#1412,.T.);
#3734=EDGE_CURVE('',#2889,#2890,#1880,.T.);
#3735=EDGE_CURVE('',#2889,#2887,#1413,.T.);
#3736=EDGE_CURVE('',#2890,#2888,#1414,.T.);
#3737=EDGE_CURVE('',#2891,#2892,#1881,.T.);
#3738=EDGE_CURVE('',#2891,#2889,#1415,.T.);
#3739=EDGE_CURVE('',#2892,#2890,#1416,.T.);
#3740=EDGE_CURVE('',#2893,#2894,#1882,.T.);
#3741=EDGE_CURVE('',#2893,#2891,#1417,.T.);
#3742=EDGE_CURVE('',#2894,#2892,#1418,.T.);
#3743=EDGE_CURVE('',#2895,#2896,#1883,.T.);
#3744=EDGE_CURVE('',#2895,#2893,#1419,.T.);
#3745=EDGE_CURVE('',#2896,#2894,#1420,.T.);
#3746=EDGE_CURVE('',#2897,#2898,#1884,.T.);
#3747=EDGE_CURVE('',#2897,#2895,#1421,.T.);
#3748=EDGE_CURVE('',#2898,#2896,#1422,.T.);
#3749=EDGE_CURVE('',#2880,#2899,#1423,.T.);
#3750=EDGE_CURVE('',#2900,#2879,#1424,.T.);
#3751=EDGE_CURVE('',#2901,#2900,#1142,.T.);
#3752=EDGE_CURVE('',#2899,#2901,#1425,.T.);
#3753=EDGE_CURVE('',#2899,#2902,#1885,.T.);
#3754=EDGE_CURVE('',#2902,#2902,#1143,.T.);
#3755=EDGE_CURVE('',#2903,#2897,#1426,.T.);
#3756=EDGE_CURVE('',#2857,#2903,#1427,.T.);
#3757=EDGE_CURVE('',#2900,#2875,#1428,.T.);
#3758=EDGE_CURVE('',#2904,#2898,#1429,.T.);
#3759=EDGE_CURVE('',#2903,#2904,#1144,.T.);
#3760=EDGE_CURVE('',#2876,#2901,#1430,.T.);
#3761=EDGE_CURVE('',#2904,#2858,#1431,.T.);
#3762=EDGE_CURVE('',#2905,#2906,#1886,.T.);
#3763=EDGE_CURVE('',#2905,#2907,#1887,.T.);
#3764=EDGE_CURVE('',#2907,#2908,#1888,.T.);
#3765=EDGE_CURVE('',#2906,#2908,#1889,.T.);
#3766=EDGE_CURVE('',#2909,#2905,#1890,.T.);
#3767=EDGE_CURVE('',#2909,#2910,#1891,.T.);
#3768=EDGE_CURVE('',#2910,#2907,#1892,.T.);
#3769=EDGE_CURVE('',#2911,#2909,#1893,.T.);
#3770=EDGE_CURVE('',#2911,#2912,#1894,.T.);
#3771=EDGE_CURVE('',#2912,#2910,#1895,.T.);
#3772=EDGE_CURVE('',#2913,#2911,#1896,.T.);
#3773=EDGE_CURVE('',#2913,#2914,#1897,.T.);
#3774=EDGE_CURVE('',#2914,#2912,#1898,.T.);
#3775=EDGE_CURVE('',#2915,#2913,#1899,.T.);
#3776=EDGE_CURVE('',#2915,#2916,#1900,.T.);
#3777=EDGE_CURVE('',#2916,#2914,#1901,.T.);
#3778=EDGE_CURVE('',#2906,#2915,#1902,.T.);
#3779=EDGE_CURVE('',#2908,#2916,#1903,.T.);
#3780=EDGE_CURVE('',#2917,#2917,#1145,.T.);
#3781=EDGE_CURVE('',#2917,#2918,#1904,.T.);
#3782=EDGE_CURVE('',#2918,#2918,#1146,.T.);
#3783=EDGE_CURVE('',#2919,#2920,#1905,.T.);
#3784=EDGE_CURVE('',#2919,#2921,#1432,.T.);
#3785=EDGE_CURVE('',#2921,#2922,#1147,.F.);
#3786=EDGE_CURVE('',#2922,#2920,#1433,.T.);
#3787=EDGE_CURVE('',#2923,#2924,#1906,.T.);
#3788=EDGE_CURVE('',#2923,#2919,#1434,.T.);
#3789=EDGE_CURVE('',#2920,#2924,#1435,.T.);
#3790=EDGE_CURVE('',#2925,#2926,#1907,.T.);
#3791=EDGE_CURVE('',#2925,#2923,#1436,.T.);
#3792=EDGE_CURVE('',#2924,#2926,#1437,.T.);
#3793=EDGE_CURVE('',#2927,#2928,#1908,.T.);
#3794=EDGE_CURVE('',#2927,#2925,#1438,.T.);
#3795=EDGE_CURVE('',#2926,#2928,#1439,.T.);
#3796=EDGE_CURVE('',#2929,#2930,#1909,.T.);
#3797=EDGE_CURVE('',#2929,#2927,#1440,.T.);
#3798=EDGE_CURVE('',#2928,#2930,#1441,.T.);
#3799=EDGE_CURVE('',#2931,#2932,#1910,.T.);
#3800=EDGE_CURVE('',#2931,#2929,#1442,.T.);
#3801=EDGE_CURVE('',#2930,#2932,#1443,.T.);
#3802=EDGE_CURVE('',#2933,#2934,#1911,.T.);
#3803=EDGE_CURVE('',#2933,#2931,#1444,.T.);
#3804=EDGE_CURVE('',#2932,#2934,#1445,.T.);
#3805=EDGE_CURVE('',#2935,#2936,#1912,.T.);
#3806=EDGE_CURVE('',#2935,#2933,#1446,.T.);
#3807=EDGE_CURVE('',#2934,#2936,#1447,.T.);
#3808=EDGE_CURVE('',#2937,#2938,#1913,.T.);
#3809=EDGE_CURVE('',#2937,#2935,#1448,.T.);
#3810=EDGE_CURVE('',#2936,#2938,#1449,.T.);
#3811=EDGE_CURVE('',#2939,#2940,#1914,.T.);
#3812=EDGE_CURVE('',#2939,#2937,#1450,.T.);
#3813=EDGE_CURVE('',#2938,#2940,#1451,.T.);
#3814=EDGE_CURVE('',#2941,#2942,#1915,.T.);
#3815=EDGE_CURVE('',#2941,#2939,#1452,.T.);
#3816=EDGE_CURVE('',#2940,#2942,#1453,.T.);
#3817=EDGE_CURVE('',#2943,#2944,#1916,.T.);
#3818=EDGE_CURVE('',#2943,#2941,#1454,.T.);
#3819=EDGE_CURVE('',#2942,#2944,#1455,.T.);
#3820=EDGE_CURVE('',#2945,#2946,#1917,.T.);
#3821=EDGE_CURVE('',#2945,#2943,#1456,.T.);
#3822=EDGE_CURVE('',#2944,#2946,#1457,.T.);
#3823=EDGE_CURVE('',#2947,#2948,#1918,.T.);
#3824=EDGE_CURVE('',#2947,#2945,#1458,.T.);
#3825=EDGE_CURVE('',#2946,#2948,#1459,.T.);
#3826=EDGE_CURVE('',#2949,#2950,#1919,.T.);
#3827=EDGE_CURVE('',#2949,#2947,#1460,.T.);
#3828=EDGE_CURVE('',#2948,#2950,#1461,.T.);
#3829=EDGE_CURVE('',#2951,#2952,#1920,.T.);
#3830=EDGE_CURVE('',#2951,#2953,#1462,.T.);
#3831=EDGE_CURVE('',#2953,#2954,#1148,.T.);
#3832=EDGE_CURVE('',#2952,#2954,#1463,.T.);
#3833=EDGE_CURVE('',#2955,#2956,#1921,.T.);
#3834=EDGE_CURVE('',#2955,#2951,#1464,.T.);
#3835=EDGE_CURVE('',#2956,#2952,#1465,.T.);
#3836=EDGE_CURVE('',#2957,#2958,#1922,.T.);
#3837=EDGE_CURVE('',#2957,#2955,#1466,.T.);
#3838=EDGE_CURVE('',#2958,#2956,#1467,.T.);
#3839=EDGE_CURVE('',#2959,#2960,#1923,.T.);
#3840=EDGE_CURVE('',#2959,#2957,#1468,.T.);
#3841=EDGE_CURVE('',#2960,#2958,#1469,.T.);
#3842=EDGE_CURVE('',#2961,#2962,#1924,.T.);
#3843=EDGE_CURVE('',#2961,#2959,#1470,.T.);
#3844=EDGE_CURVE('',#2962,#2960,#1471,.T.);
#3845=EDGE_CURVE('',#2963,#2964,#1925,.T.);
#3846=EDGE_CURVE('',#2963,#2961,#1472,.T.);
#3847=EDGE_CURVE('',#2964,#2962,#1473,.T.);
#3848=EDGE_CURVE('',#2965,#2966,#1926,.T.);
#3849=EDGE_CURVE('',#2965,#2963,#1474,.T.);
#3850=EDGE_CURVE('',#2966,#2964,#1475,.T.);
#3851=EDGE_CURVE('',#2967,#2968,#1927,.T.);
#3852=EDGE_CURVE('',#2967,#2965,#1476,.T.);
#3853=EDGE_CURVE('',#2968,#2966,#1477,.T.);
#3854=EDGE_CURVE('',#2969,#2970,#1928,.T.);
#3855=EDGE_CURVE('',#2969,#2967,#1478,.T.);
#3856=EDGE_CURVE('',#2970,#2968,#1479,.T.);
#3857=EDGE_CURVE('',#2971,#2972,#1929,.T.);
#3858=EDGE_CURVE('',#2971,#2969,#1480,.T.);
#3859=EDGE_CURVE('',#2972,#2970,#1481,.T.);
#3860=EDGE_CURVE('',#2973,#2974,#1930,.T.);
#3861=EDGE_CURVE('',#2973,#2971,#1482,.T.);
#3862=EDGE_CURVE('',#2974,#2972,#1483,.T.);
#3863=EDGE_CURVE('',#2975,#2976,#1931,.T.);
#3864=EDGE_CURVE('',#2975,#2973,#1484,.T.);
#3865=EDGE_CURVE('',#2976,#2974,#1485,.T.);
#3866=EDGE_CURVE('',#2977,#2978,#1932,.T.);
#3867=EDGE_CURVE('',#2977,#2975,#1486,.T.);
#3868=EDGE_CURVE('',#2978,#2976,#1487,.T.);
#3869=EDGE_CURVE('',#2979,#2980,#1933,.T.);
#3870=EDGE_CURVE('',#2979,#2977,#1488,.T.);
#3871=EDGE_CURVE('',#2980,#2978,#1489,.T.);
#3872=EDGE_CURVE('',#2981,#2982,#1934,.T.);
#3873=EDGE_CURVE('',#2981,#2979,#1490,.T.);
#3874=EDGE_CURVE('',#2982,#2980,#1491,.T.);
#3875=EDGE_CURVE('',#2954,#2983,#1492,.T.);
#3876=EDGE_CURVE('',#2984,#2953,#1493,.T.);
#3877=EDGE_CURVE('',#2985,#2984,#1149,.T.);
#3878=EDGE_CURVE('',#2983,#2985,#1494,.T.);
#3879=EDGE_CURVE('',#2983,#2986,#1935,.T.);
#3880=EDGE_CURVE('',#2986,#2986,#1150,.T.);
#3881=EDGE_CURVE('',#2987,#2981,#1495,.T.);
#3882=EDGE_CURVE('',#2921,#2987,#1496,.T.);
#3883=EDGE_CURVE('',#2984,#2949,#1497,.T.);
#3884=EDGE_CURVE('',#2988,#2982,#1498,.T.);
#3885=EDGE_CURVE('',#2987,#2988,#1151,.T.);
#3886=EDGE_CURVE('',#2950,#2985,#1499,.T.);
#3887=EDGE_CURVE('',#2988,#2922,#1500,.T.);
#3888=EDGE_CURVE('',#2989,#2990,#1936,.T.);
#3889=EDGE_CURVE('',#2989,#2991,#1937,.T.);
#3890=EDGE_CURVE('',#2991,#2992,#1938,.T.);
#3891=EDGE_CURVE('',#2990,#2992,#1939,.T.);
#3892=EDGE_CURVE('',#2993,#2989,#1940,.T.);
#3893=EDGE_CURVE('',#2993,#2994,#1941,.T.);
#3894=EDGE_CURVE('',#2994,#2991,#1942,.T.);
#3895=EDGE_CURVE('',#2995,#2993,#1943,.T.);
#3896=EDGE_CURVE('',#2995,#2996,#1944,.T.);
#3897=EDGE_CURVE('',#2996,#2994,#1945,.T.);
#3898=EDGE_CURVE('',#2997,#2995,#1946,.T.);
#3899=EDGE_CURVE('',#2997,#2998,#1947,.T.);
#3900=EDGE_CURVE('',#2998,#2996,#1948,.T.);
#3901=EDGE_CURVE('',#2999,#2997,#1949,.T.);
#3902=EDGE_CURVE('',#2999,#3000,#1950,.T.);
#3903=EDGE_CURVE('',#3000,#2998,#1951,.T.);
#3904=EDGE_CURVE('',#2990,#2999,#1952,.T.);
#3905=EDGE_CURVE('',#2992,#3000,#1953,.T.);
#3906=EDGE_CURVE('',#3001,#3001,#1152,.T.);
#3907=EDGE_CURVE('',#3001,#3002,#1954,.T.);
#3908=EDGE_CURVE('',#3002,#3002,#1153,.T.);
#3909=EDGE_CURVE('',#3003,#3003,#1154,.T.);
#3910=EDGE_CURVE('',#3003,#3004,#1955,.T.);
#3911=EDGE_CURVE('',#3004,#3004,#1155,.T.);
#3912=EDGE_CURVE('',#3005,#3005,#1156,.T.);
#3913=EDGE_CURVE('',#3005,#3006,#1956,.T.);
#3914=EDGE_CURVE('',#3006,#3006,#1157,.T.);
#3915=EDGE_CURVE('',#3007,#3008,#1957,.T.);
#3916=EDGE_CURVE('',#3008,#3009,#1501,.T.);
#3917=EDGE_CURVE('',#3010,#3009,#1158,.F.);
#3918=EDGE_CURVE('',#3010,#3007,#1502,.T.);
#3919=EDGE_CURVE('',#3011,#3012,#1958,.T.);
#3920=EDGE_CURVE('',#3012,#3008,#1503,.T.);
#3921=EDGE_CURVE('',#3007,#3011,#1504,.T.);
#3922=EDGE_CURVE('',#3013,#3014,#1959,.T.);
#3923=EDGE_CURVE('',#3014,#3012,#1505,.T.);
#3924=EDGE_CURVE('',#3011,#3013,#1506,.T.);
#3925=EDGE_CURVE('',#3015,#3016,#1960,.T.);
#3926=EDGE_CURVE('',#3016,#3014,#1507,.T.);
#3927=EDGE_CURVE('',#3013,#3015,#1508,.T.);
#3928=EDGE_CURVE('',#3017,#3018,#1961,.T.);
#3929=EDGE_CURVE('',#3017,#3019,#1509,.T.);
#3930=EDGE_CURVE('',#3020,#3019,#1159,.T.);
#3931=EDGE_CURVE('',#3020,#3018,#1510,.T.);
#3932=EDGE_CURVE('',#3021,#3022,#1962,.T.);
#3933=EDGE_CURVE('',#3022,#3023,#1511,.T.);
#3934=EDGE_CURVE('',#3024,#3023,#1160,.T.);
#3935=EDGE_CURVE('',#3021,#3024,#1512,.T.);
#3936=EDGE_CURVE('',#3025,#3026,#1963,.T.);
#3937=EDGE_CURVE('',#3026,#3022,#1513,.T.);
#3938=EDGE_CURVE('',#3025,#3021,#1514,.T.);
#3939=EDGE_CURVE('',#3027,#3028,#1964,.T.);
#3940=EDGE_CURVE('',#3028,#3026,#1515,.T.);
#3941=EDGE_CURVE('',#3027,#3025,#1516,.T.);
#3942=EDGE_CURVE('',#3029,#3030,#1965,.T.);
#3943=EDGE_CURVE('',#3030,#3028,#1517,.T.);
#3944=EDGE_CURVE('',#3029,#3027,#1518,.T.);
#3945=EDGE_CURVE('',#3031,#3032,#1966,.T.);
#3946=EDGE_CURVE('',#3033,#3031,#1519,.T.);
#3947=EDGE_CURVE('',#3034,#3033,#1161,.T.);
#3948=EDGE_CURVE('',#3034,#3032,#1520,.T.);
#3949=EDGE_CURVE('',#3032,#3030,#1521,.T.);
#3950=EDGE_CURVE('',#3031,#3029,#1522,.T.);
#3951=EDGE_CURVE('',#3023,#3010,#1523,.T.);
#3952=EDGE_CURVE('',#3019,#3034,#1524,.T.);
#3953=EDGE_CURVE('',#3015,#3017,#1525,.T.);
#3954=EDGE_CURVE('',#3009,#3024,#1526,.T.);
#3955=EDGE_CURVE('',#3018,#3016,#1527,.T.);
#3956=EDGE_CURVE('',#3033,#3020,#1528,.T.);
#3957=EDGE_CURVE('',#3035,#3036,#1967,.T.);
#3958=EDGE_CURVE('',#3036,#3037,#1968,.T.);
#3959=EDGE_CURVE('',#3037,#3038,#1969,.T.);
#3960=EDGE_CURVE('',#3038,#3039,#1970,.T.);
#3961=EDGE_CURVE('',#3039,#3040,#1971,.T.);
#3962=EDGE_CURVE('',#3040,#3035,#1972,.T.);
#3963=EDGE_CURVE('',#3041,#3042,#1973,.T.);
#3964=EDGE_CURVE('',#3042,#3035,#1974,.T.);
#3965=EDGE_CURVE('',#3041,#3040,#1975,.T.);
#3966=EDGE_CURVE('',#3043,#3041,#1976,.T.);
#3967=EDGE_CURVE('',#3043,#3039,#1977,.T.);
#3968=EDGE_CURVE('',#3044,#3043,#1978,.T.);
#3969=EDGE_CURVE('',#3044,#3038,#1979,.T.);
#3970=EDGE_CURVE('',#3045,#3044,#1980,.T.);
#3971=EDGE_CURVE('',#3045,#3037,#1981,.T.);
#3972=EDGE_CURVE('',#3046,#3045,#1982,.T.);
#3973=EDGE_CURVE('',#3046,#3036,#1983,.T.);
#3974=EDGE_CURVE('',#3042,#3046,#1984,.T.);
#3975=ORIENTED_EDGE('',*,*,#3047,.T.);
#3976=ORIENTED_EDGE('',*,*,#3048,.T.);
#3977=ORIENTED_EDGE('',*,*,#3049,.F.);
#3978=ORIENTED_EDGE('',*,*,#3050,.T.);
#3979=ORIENTED_EDGE('',*,*,#3051,.T.);
#3980=ORIENTED_EDGE('',*,*,#3052,.T.);
#3981=ORIENTED_EDGE('',*,*,#3047,.F.);
#3982=ORIENTED_EDGE('',*,*,#3053,.T.);
#3983=ORIENTED_EDGE('',*,*,#3054,.T.);
#3984=ORIENTED_EDGE('',*,*,#3055,.T.);
#3985=ORIENTED_EDGE('',*,*,#3051,.F.);
#3986=ORIENTED_EDGE('',*,*,#3056,.T.);
#3987=ORIENTED_EDGE('',*,*,#3057,.T.);
#3988=ORIENTED_EDGE('',*,*,#3058,.T.);
#3989=ORIENTED_EDGE('',*,*,#3054,.F.);
#3990=ORIENTED_EDGE('',*,*,#3059,.T.);
#3991=ORIENTED_EDGE('',*,*,#3060,.T.);
#3992=ORIENTED_EDGE('',*,*,#3061,.T.);
#3993=ORIENTED_EDGE('',*,*,#3057,.F.);
#3994=ORIENTED_EDGE('',*,*,#3062,.T.);
#3995=ORIENTED_EDGE('',*,*,#3063,.T.);
#3996=ORIENTED_EDGE('',*,*,#3064,.T.);
#3997=ORIENTED_EDGE('',*,*,#3060,.F.);
#3998=ORIENTED_EDGE('',*,*,#3065,.T.);
#3999=ORIENTED_EDGE('',*,*,#3066,.T.);
#4000=ORIENTED_EDGE('',*,*,#3067,.T.);
#4001=ORIENTED_EDGE('',*,*,#3063,.F.);
#4002=ORIENTED_EDGE('',*,*,#3068,.T.);
#4003=ORIENTED_EDGE('',*,*,#3069,.T.);
#4004=ORIENTED_EDGE('',*,*,#3070,.T.);
#4005=ORIENTED_EDGE('',*,*,#3066,.F.);
#4006=ORIENTED_EDGE('',*,*,#3071,.T.);
#4007=ORIENTED_EDGE('',*,*,#3072,.T.);
#4008=ORIENTED_EDGE('',*,*,#3073,.T.);
#4009=ORIENTED_EDGE('',*,*,#3069,.F.);
#4010=ORIENTED_EDGE('',*,*,#3074,.T.);
#4011=ORIENTED_EDGE('',*,*,#3075,.T.);
#4012=ORIENTED_EDGE('',*,*,#3076,.T.);
#4013=ORIENTED_EDGE('',*,*,#3072,.F.);
#4014=ORIENTED_EDGE('',*,*,#3077,.T.);
#4015=ORIENTED_EDGE('',*,*,#3078,.F.);
#4016=ORIENTED_EDGE('',*,*,#3079,.T.);
#4017=ORIENTED_EDGE('',*,*,#3080,.T.);
#4018=ORIENTED_EDGE('',*,*,#3081,.T.);
#4019=ORIENTED_EDGE('',*,*,#3082,.T.);
#4020=ORIENTED_EDGE('',*,*,#3083,.T.);
#4021=ORIENTED_EDGE('',*,*,#3084,.F.);
#4022=ORIENTED_EDGE('',*,*,#3085,.T.);
#4023=ORIENTED_EDGE('',*,*,#3086,.T.);
#4024=ORIENTED_EDGE('',*,*,#3087,.T.);
#4025=ORIENTED_EDGE('',*,*,#3082,.F.);
#4026=ORIENTED_EDGE('',*,*,#3088,.T.);
#4027=ORIENTED_EDGE('',*,*,#3089,.T.);
#4028=ORIENTED_EDGE('',*,*,#3090,.T.);
#4029=ORIENTED_EDGE('',*,*,#3086,.F.);
#4030=ORIENTED_EDGE('',*,*,#3091,.T.);
#4031=ORIENTED_EDGE('',*,*,#3092,.T.);
#4032=ORIENTED_EDGE('',*,*,#3093,.T.);
#4033=ORIENTED_EDGE('',*,*,#3089,.F.);
#4034=ORIENTED_EDGE('',*,*,#3094,.T.);
#4035=ORIENTED_EDGE('',*,*,#3095,.T.);
#4036=ORIENTED_EDGE('',*,*,#3096,.T.);
#4037=ORIENTED_EDGE('',*,*,#3092,.F.);
#4038=ORIENTED_EDGE('',*,*,#3097,.T.);
#4039=ORIENTED_EDGE('',*,*,#3098,.T.);
#4040=ORIENTED_EDGE('',*,*,#3099,.T.);
#4041=ORIENTED_EDGE('',*,*,#3095,.F.);
#4042=ORIENTED_EDGE('',*,*,#3100,.T.);
#4043=ORIENTED_EDGE('',*,*,#3101,.T.);
#4044=ORIENTED_EDGE('',*,*,#3102,.T.);
#4045=ORIENTED_EDGE('',*,*,#3098,.F.);
#4046=ORIENTED_EDGE('',*,*,#3103,.T.);
#4047=ORIENTED_EDGE('',*,*,#3104,.T.);
#4048=ORIENTED_EDGE('',*,*,#3105,.T.);
#4049=ORIENTED_EDGE('',*,*,#3101,.F.);
#4050=ORIENTED_EDGE('',*,*,#3106,.T.);
#4051=ORIENTED_EDGE('',*,*,#3107,.T.);
#4052=ORIENTED_EDGE('',*,*,#3108,.T.);
#4053=ORIENTED_EDGE('',*,*,#3104,.F.);
#4054=ORIENTED_EDGE('',*,*,#3109,.T.);
#4055=ORIENTED_EDGE('',*,*,#3110,.T.);
#4056=ORIENTED_EDGE('',*,*,#3111,.T.);
#4057=ORIENTED_EDGE('',*,*,#3107,.F.);
#4058=ORIENTED_EDGE('',*,*,#3112,.T.);
#4059=ORIENTED_EDGE('',*,*,#3113,.F.);
#4060=ORIENTED_EDGE('',*,*,#3114,.T.);
#4061=ORIENTED_EDGE('',*,*,#3115,.T.);
#4062=ORIENTED_EDGE('',*,*,#3116,.T.);
#4063=ORIENTED_EDGE('',*,*,#3117,.T.);
#4064=ORIENTED_EDGE('',*,*,#3118,.T.);
#4065=ORIENTED_EDGE('',*,*,#3119,.F.);
#4066=ORIENTED_EDGE('',*,*,#3120,.T.);
#4067=ORIENTED_EDGE('',*,*,#3121,.T.);
#4068=ORIENTED_EDGE('',*,*,#3122,.T.);
#4069=ORIENTED_EDGE('',*,*,#3117,.F.);
#4070=ORIENTED_EDGE('',*,*,#3123,.T.);
#4071=ORIENTED_EDGE('',*,*,#3124,.T.);
#4072=ORIENTED_EDGE('',*,*,#3125,.T.);
#4073=ORIENTED_EDGE('',*,*,#3121,.F.);
#4074=ORIENTED_EDGE('',*,*,#3126,.T.);
#4075=ORIENTED_EDGE('',*,*,#3127,.T.);
#4076=ORIENTED_EDGE('',*,*,#3128,.T.);
#4077=ORIENTED_EDGE('',*,*,#3124,.F.);
#4078=ORIENTED_EDGE('',*,*,#3129,.T.);
#4079=ORIENTED_EDGE('',*,*,#3130,.T.);
#4080=ORIENTED_EDGE('',*,*,#3131,.T.);
#4081=ORIENTED_EDGE('',*,*,#3127,.F.);
#4082=ORIENTED_EDGE('',*,*,#3132,.T.);
#4083=ORIENTED_EDGE('',*,*,#3133,.T.);
#4084=ORIENTED_EDGE('',*,*,#3134,.T.);
#4085=ORIENTED_EDGE('',*,*,#3130,.F.);
#4086=ORIENTED_EDGE('',*,*,#3135,.T.);
#4087=ORIENTED_EDGE('',*,*,#3136,.T.);
#4088=ORIENTED_EDGE('',*,*,#3137,.T.);
#4089=ORIENTED_EDGE('',*,*,#3133,.F.);
#4090=ORIENTED_EDGE('',*,*,#3138,.T.);
#4091=ORIENTED_EDGE('',*,*,#3139,.T.);
#4092=ORIENTED_EDGE('',*,*,#3140,.T.);
#4093=ORIENTED_EDGE('',*,*,#3136,.F.);
#4094=ORIENTED_EDGE('',*,*,#3141,.T.);
#4095=ORIENTED_EDGE('',*,*,#3142,.T.);
#4096=ORIENTED_EDGE('',*,*,#3143,.T.);
#4097=ORIENTED_EDGE('',*,*,#3139,.F.);
#4098=ORIENTED_EDGE('',*,*,#3144,.T.);
#4099=ORIENTED_EDGE('',*,*,#3145,.T.);
#4100=ORIENTED_EDGE('',*,*,#3146,.T.);
#4101=ORIENTED_EDGE('',*,*,#3142,.F.);
#4102=ORIENTED_EDGE('',*,*,#3147,.T.);
#4103=ORIENTED_EDGE('',*,*,#3148,.F.);
#4104=ORIENTED_EDGE('',*,*,#3149,.T.);
#4105=ORIENTED_EDGE('',*,*,#3150,.F.);
#4106=ORIENTED_EDGE('',*,*,#3151,.T.);
#4107=ORIENTED_EDGE('',*,*,#3152,.T.);
#4108=ORIENTED_EDGE('',*,*,#3153,.T.);
#4109=ORIENTED_EDGE('',*,*,#3154,.T.);
#4110=ORIENTED_EDGE('',*,*,#3155,.F.);
#4111=ORIENTED_EDGE('',*,*,#3156,.T.);
#4112=ORIENTED_EDGE('',*,*,#3157,.T.);
#4113=ORIENTED_EDGE('',*,*,#3158,.T.);
#4114=ORIENTED_EDGE('',*,*,#3153,.F.);
#4115=ORIENTED_EDGE('',*,*,#3159,.T.);
#4116=ORIENTED_EDGE('',*,*,#3160,.T.);
#4117=ORIENTED_EDGE('',*,*,#3161,.T.);
#4118=ORIENTED_EDGE('',*,*,#3157,.F.);
#4119=ORIENTED_EDGE('',*,*,#3162,.T.);
#4120=ORIENTED_EDGE('',*,*,#3163,.T.);
#4121=ORIENTED_EDGE('',*,*,#3164,.T.);
#4122=ORIENTED_EDGE('',*,*,#3160,.F.);
#4123=ORIENTED_EDGE('',*,*,#3165,.T.);
#4124=ORIENTED_EDGE('',*,*,#3166,.T.);
#4125=ORIENTED_EDGE('',*,*,#3167,.T.);
#4126=ORIENTED_EDGE('',*,*,#3163,.F.);
#4127=ORIENTED_EDGE('',*,*,#3168,.T.);
#4128=ORIENTED_EDGE('',*,*,#3169,.T.);
#4129=ORIENTED_EDGE('',*,*,#3170,.T.);
#4130=ORIENTED_EDGE('',*,*,#3166,.F.);
#4131=ORIENTED_EDGE('',*,*,#3171,.T.);
#4132=ORIENTED_EDGE('',*,*,#3172,.T.);
#4133=ORIENTED_EDGE('',*,*,#3173,.T.);
#4134=ORIENTED_EDGE('',*,*,#3169,.F.);
#4135=ORIENTED_EDGE('',*,*,#3174,.T.);
#4136=ORIENTED_EDGE('',*,*,#3175,.T.);
#4137=ORIENTED_EDGE('',*,*,#3176,.T.);
#4138=ORIENTED_EDGE('',*,*,#3172,.F.);
#4139=ORIENTED_EDGE('',*,*,#3177,.T.);
#4140=ORIENTED_EDGE('',*,*,#3178,.T.);
#4141=ORIENTED_EDGE('',*,*,#3179,.T.);
#4142=ORIENTED_EDGE('',*,*,#3175,.F.);
#4143=ORIENTED_EDGE('',*,*,#3180,.T.);
#4144=ORIENTED_EDGE('',*,*,#3181,.T.);
#4145=ORIENTED_EDGE('',*,*,#3182,.T.);
#4146=ORIENTED_EDGE('',*,*,#3178,.F.);
#4147=ORIENTED_EDGE('',*,*,#3183,.T.);
#4148=ORIENTED_EDGE('',*,*,#3184,.F.);
#4149=ORIENTED_EDGE('',*,*,#3185,.T.);
#4150=ORIENTED_EDGE('',*,*,#3186,.T.);
#4151=ORIENTED_EDGE('',*,*,#3187,.F.);
#4152=ORIENTED_EDGE('',*,*,#3188,.T.);
#4153=ORIENTED_EDGE('',*,*,#3189,.T.);
#4154=ORIENTED_EDGE('',*,*,#3190,.T.);
#4155=ORIENTED_EDGE('',*,*,#3191,.F.);
#4156=ORIENTED_EDGE('',*,*,#3192,.F.);
#4157=ORIENTED_EDGE('',*,*,#3193,.T.);
#4158=ORIENTED_EDGE('',*,*,#3194,.T.);
#4159=ORIENTED_EDGE('',*,*,#3189,.F.);
#4160=ORIENTED_EDGE('',*,*,#3195,.F.);
#4161=ORIENTED_EDGE('',*,*,#3196,.T.);
#4162=ORIENTED_EDGE('',*,*,#3197,.T.);
#4163=ORIENTED_EDGE('',*,*,#3193,.F.);
#4164=ORIENTED_EDGE('',*,*,#3198,.F.);
#4165=ORIENTED_EDGE('',*,*,#3199,.T.);
#4166=ORIENTED_EDGE('',*,*,#3200,.T.);
#4167=ORIENTED_EDGE('',*,*,#3196,.F.);
#4168=ORIENTED_EDGE('',*,*,#3201,.F.);
#4169=ORIENTED_EDGE('',*,*,#3202,.T.);
#4170=ORIENTED_EDGE('',*,*,#3203,.T.);
#4171=ORIENTED_EDGE('',*,*,#3199,.F.);
#4172=ORIENTED_EDGE('',*,*,#3204,.F.);
#4173=ORIENTED_EDGE('',*,*,#3205,.T.);
#4174=ORIENTED_EDGE('',*,*,#3206,.T.);
#4175=ORIENTED_EDGE('',*,*,#3202,.F.);
#4176=ORIENTED_EDGE('',*,*,#3207,.F.);
#4177=ORIENTED_EDGE('',*,*,#3208,.T.);
#4178=ORIENTED_EDGE('',*,*,#3209,.T.);
#4179=ORIENTED_EDGE('',*,*,#3205,.F.);
#4180=ORIENTED_EDGE('',*,*,#3210,.F.);
#4181=ORIENTED_EDGE('',*,*,#3211,.T.);
#4182=ORIENTED_EDGE('',*,*,#3212,.T.);
#4183=ORIENTED_EDGE('',*,*,#3208,.F.);
#4184=ORIENTED_EDGE('',*,*,#3213,.F.);
#4185=ORIENTED_EDGE('',*,*,#3214,.T.);
#4186=ORIENTED_EDGE('',*,*,#3215,.T.);
#4187=ORIENTED_EDGE('',*,*,#3211,.F.);
#4188=ORIENTED_EDGE('',*,*,#3216,.F.);
#4189=ORIENTED_EDGE('',*,*,#3217,.T.);
#4190=ORIENTED_EDGE('',*,*,#3218,.T.);
#4191=ORIENTED_EDGE('',*,*,#3214,.F.);
#4192=ORIENTED_EDGE('',*,*,#3219,.F.);
#4193=ORIENTED_EDGE('',*,*,#3220,.T.);
#4194=ORIENTED_EDGE('',*,*,#3221,.T.);
#4195=ORIENTED_EDGE('',*,*,#3217,.F.);
#4196=ORIENTED_EDGE('',*,*,#3222,.F.);
#4197=ORIENTED_EDGE('',*,*,#3223,.F.);
#4198=ORIENTED_EDGE('',*,*,#3224,.F.);
#4199=ORIENTED_EDGE('',*,*,#3225,.F.);
#4200=ORIENTED_EDGE('',*,*,#3226,.T.);
#4201=ORIENTED_EDGE('',*,*,#3227,.T.);
#4202=ORIENTED_EDGE('',*,*,#3228,.T.);
#4203=ORIENTED_EDGE('',*,*,#3229,.F.);
#4204=ORIENTED_EDGE('',*,*,#3230,.F.);
#4205=ORIENTED_EDGE('',*,*,#3231,.T.);
#4206=ORIENTED_EDGE('',*,*,#3232,.T.);
#4207=ORIENTED_EDGE('',*,*,#3227,.F.);
#4208=ORIENTED_EDGE('',*,*,#3233,.F.);
#4209=ORIENTED_EDGE('',*,*,#3234,.T.);
#4210=ORIENTED_EDGE('',*,*,#3235,.T.);
#4211=ORIENTED_EDGE('',*,*,#3231,.F.);
#4212=ORIENTED_EDGE('',*,*,#3236,.F.);
#4213=ORIENTED_EDGE('',*,*,#3237,.T.);
#4214=ORIENTED_EDGE('',*,*,#3238,.T.);
#4215=ORIENTED_EDGE('',*,*,#3234,.F.);
#4216=ORIENTED_EDGE('',*,*,#3239,.F.);
#4217=ORIENTED_EDGE('',*,*,#3240,.T.);
#4218=ORIENTED_EDGE('',*,*,#3241,.T.);
#4219=ORIENTED_EDGE('',*,*,#3237,.F.);
#4220=ORIENTED_EDGE('',*,*,#3242,.F.);
#4221=ORIENTED_EDGE('',*,*,#3243,.T.);
#4222=ORIENTED_EDGE('',*,*,#3244,.T.);
#4223=ORIENTED_EDGE('',*,*,#3240,.F.);
#4224=ORIENTED_EDGE('',*,*,#3245,.F.);
#4225=ORIENTED_EDGE('',*,*,#3246,.T.);
#4226=ORIENTED_EDGE('',*,*,#3247,.T.);
#4227=ORIENTED_EDGE('',*,*,#3243,.F.);
#4228=ORIENTED_EDGE('',*,*,#3248,.F.);
#4229=ORIENTED_EDGE('',*,*,#3249,.T.);
#4230=ORIENTED_EDGE('',*,*,#3250,.T.);
#4231=ORIENTED_EDGE('',*,*,#3246,.F.);
#4232=ORIENTED_EDGE('',*,*,#3251,.F.);
#4233=ORIENTED_EDGE('',*,*,#3252,.T.);
#4234=ORIENTED_EDGE('',*,*,#3253,.T.);
#4235=ORIENTED_EDGE('',*,*,#3249,.F.);
#4236=ORIENTED_EDGE('',*,*,#3254,.F.);
#4237=ORIENTED_EDGE('',*,*,#3255,.T.);
#4238=ORIENTED_EDGE('',*,*,#3256,.T.);
#4239=ORIENTED_EDGE('',*,*,#3252,.F.);
#4240=ORIENTED_EDGE('',*,*,#3257,.F.);
#4241=ORIENTED_EDGE('',*,*,#3258,.T.);
#4242=ORIENTED_EDGE('',*,*,#3259,.T.);
#4243=ORIENTED_EDGE('',*,*,#3255,.F.);
#4244=ORIENTED_EDGE('',*,*,#3260,.F.);
#4245=ORIENTED_EDGE('',*,*,#3261,.F.);
#4246=ORIENTED_EDGE('',*,*,#3262,.F.);
#4247=ORIENTED_EDGE('',*,*,#3263,.F.);
#4248=ORIENTED_EDGE('',*,*,#3264,.T.);
#4249=ORIENTED_EDGE('',*,*,#3265,.T.);
#4250=ORIENTED_EDGE('',*,*,#3266,.T.);
#4251=ORIENTED_EDGE('',*,*,#3267,.F.);
#4252=ORIENTED_EDGE('',*,*,#3268,.F.);
#4253=ORIENTED_EDGE('',*,*,#3269,.T.);
#4254=ORIENTED_EDGE('',*,*,#3270,.T.);
#4255=ORIENTED_EDGE('',*,*,#3265,.F.);
#4256=ORIENTED_EDGE('',*,*,#3271,.F.);
#4257=ORIENTED_EDGE('',*,*,#3272,.T.);
#4258=ORIENTED_EDGE('',*,*,#3273,.T.);
#4259=ORIENTED_EDGE('',*,*,#3269,.F.);
#4260=ORIENTED_EDGE('',*,*,#3274,.F.);
#4261=ORIENTED_EDGE('',*,*,#3275,.T.);
#4262=ORIENTED_EDGE('',*,*,#3276,.T.);
#4263=ORIENTED_EDGE('',*,*,#3272,.F.);
#4264=ORIENTED_EDGE('',*,*,#3277,.F.);
#4265=ORIENTED_EDGE('',*,*,#3278,.T.);
#4266=ORIENTED_EDGE('',*,*,#3279,.T.);
#4267=ORIENTED_EDGE('',*,*,#3275,.F.);
#4268=ORIENTED_EDGE('',*,*,#3280,.F.);
#4269=ORIENTED_EDGE('',*,*,#3281,.T.);
#4270=ORIENTED_EDGE('',*,*,#3282,.T.);
#4271=ORIENTED_EDGE('',*,*,#3278,.F.);
#4272=ORIENTED_EDGE('',*,*,#3283,.F.);
#4273=ORIENTED_EDGE('',*,*,#3284,.T.);
#4274=ORIENTED_EDGE('',*,*,#3285,.T.);
#4275=ORIENTED_EDGE('',*,*,#3281,.F.);
#4276=ORIENTED_EDGE('',*,*,#3286,.F.);
#4277=ORIENTED_EDGE('',*,*,#3287,.T.);
#4278=ORIENTED_EDGE('',*,*,#3288,.T.);
#4279=ORIENTED_EDGE('',*,*,#3284,.F.);
#4280=ORIENTED_EDGE('',*,*,#3289,.F.);
#4281=ORIENTED_EDGE('',*,*,#3290,.T.);
#4282=ORIENTED_EDGE('',*,*,#3291,.T.);
#4283=ORIENTED_EDGE('',*,*,#3287,.F.);
#4284=ORIENTED_EDGE('',*,*,#3292,.F.);
#4285=ORIENTED_EDGE('',*,*,#3293,.T.);
#4286=ORIENTED_EDGE('',*,*,#3294,.T.);
#4287=ORIENTED_EDGE('',*,*,#3290,.F.);
#4288=ORIENTED_EDGE('',*,*,#3295,.F.);
#4289=ORIENTED_EDGE('',*,*,#3296,.T.);
#4290=ORIENTED_EDGE('',*,*,#3297,.T.);
#4291=ORIENTED_EDGE('',*,*,#3293,.F.);
#4292=ORIENTED_EDGE('',*,*,#3298,.F.);
#4293=ORIENTED_EDGE('',*,*,#3299,.F.);
#4294=ORIENTED_EDGE('',*,*,#3300,.F.);
#4295=ORIENTED_EDGE('',*,*,#3301,.F.);
#4296=ORIENTED_EDGE('',*,*,#3302,.T.);
#4297=ORIENTED_EDGE('',*,*,#3303,.T.);
#4298=ORIENTED_EDGE('',*,*,#3304,.T.);
#4299=ORIENTED_EDGE('',*,*,#3305,.F.);
#4300=ORIENTED_EDGE('',*,*,#3306,.F.);
#4301=ORIENTED_EDGE('',*,*,#3307,.T.);
#4302=ORIENTED_EDGE('',*,*,#3308,.T.);
#4303=ORIENTED_EDGE('',*,*,#3303,.F.);
#4304=ORIENTED_EDGE('',*,*,#3309,.F.);
#4305=ORIENTED_EDGE('',*,*,#3310,.T.);
#4306=ORIENTED_EDGE('',*,*,#3311,.T.);
#4307=ORIENTED_EDGE('',*,*,#3307,.F.);
#4308=ORIENTED_EDGE('',*,*,#3312,.F.);
#4309=ORIENTED_EDGE('',*,*,#3313,.T.);
#4310=ORIENTED_EDGE('',*,*,#3314,.T.);
#4311=ORIENTED_EDGE('',*,*,#3310,.F.);
#4312=ORIENTED_EDGE('',*,*,#3315,.F.);
#4313=ORIENTED_EDGE('',*,*,#3316,.T.);
#4314=ORIENTED_EDGE('',*,*,#3317,.T.);
#4315=ORIENTED_EDGE('',*,*,#3313,.F.);
#4316=ORIENTED_EDGE('',*,*,#3318,.F.);
#4317=ORIENTED_EDGE('',*,*,#3319,.T.);
#4318=ORIENTED_EDGE('',*,*,#3320,.T.);
#4319=ORIENTED_EDGE('',*,*,#3316,.F.);
#4320=ORIENTED_EDGE('',*,*,#3321,.F.);
#4321=ORIENTED_EDGE('',*,*,#3322,.T.);
#4322=ORIENTED_EDGE('',*,*,#3323,.T.);
#4323=ORIENTED_EDGE('',*,*,#3319,.F.);
#4324=ORIENTED_EDGE('',*,*,#3324,.F.);
#4325=ORIENTED_EDGE('',*,*,#3325,.T.);
#4326=ORIENTED_EDGE('',*,*,#3326,.T.);
#4327=ORIENTED_EDGE('',*,*,#3322,.F.);
#4328=ORIENTED_EDGE('',*,*,#3327,.F.);
#4329=ORIENTED_EDGE('',*,*,#3328,.T.);
#4330=ORIENTED_EDGE('',*,*,#3329,.T.);
#4331=ORIENTED_EDGE('',*,*,#3325,.F.);
#4332=ORIENTED_EDGE('',*,*,#3330,.F.);
#4333=ORIENTED_EDGE('',*,*,#3331,.T.);
#4334=ORIENTED_EDGE('',*,*,#3332,.T.);
#4335=ORIENTED_EDGE('',*,*,#3328,.F.);
#4336=ORIENTED_EDGE('',*,*,#3333,.F.);
#4337=ORIENTED_EDGE('',*,*,#3334,.T.);
#4338=ORIENTED_EDGE('',*,*,#3335,.T.);
#4339=ORIENTED_EDGE('',*,*,#3331,.F.);
#4340=ORIENTED_EDGE('',*,*,#3336,.F.);
#4341=ORIENTED_EDGE('',*,*,#3337,.F.);
#4342=ORIENTED_EDGE('',*,*,#3338,.F.);
#4343=ORIENTED_EDGE('',*,*,#3339,.F.);
#4344=ORIENTED_EDGE('',*,*,#3340,.T.);
#4345=ORIENTED_EDGE('',*,*,#3341,.T.);
#4346=ORIENTED_EDGE('',*,*,#3342,.T.);
#4347=ORIENTED_EDGE('',*,*,#3343,.T.);
#4348=ORIENTED_EDGE('',*,*,#3344,.F.);
#4349=ORIENTED_EDGE('',*,*,#3345,.T.);
#4350=ORIENTED_EDGE('',*,*,#3346,.T.);
#4351=ORIENTED_EDGE('',*,*,#3347,.T.);
#4352=ORIENTED_EDGE('',*,*,#3342,.F.);
#4353=ORIENTED_EDGE('',*,*,#3348,.T.);
#4354=ORIENTED_EDGE('',*,*,#3349,.T.);
#4355=ORIENTED_EDGE('',*,*,#3350,.T.);
#4356=ORIENTED_EDGE('',*,*,#3346,.F.);
#4357=ORIENTED_EDGE('',*,*,#3351,.T.);
#4358=ORIENTED_EDGE('',*,*,#3352,.T.);
#4359=ORIENTED_EDGE('',*,*,#3353,.T.);
#4360=ORIENTED_EDGE('',*,*,#3349,.F.);
#4361=ORIENTED_EDGE('',*,*,#3354,.T.);
#4362=ORIENTED_EDGE('',*,*,#3352,.F.);
#4363=ORIENTED_EDGE('',*,*,#3355,.T.);
#4364=ORIENTED_EDGE('',*,*,#3356,.T.);
#4365=ORIENTED_EDGE('',*,*,#3357,.T.);
#4366=ORIENTED_EDGE('',*,*,#3356,.F.);
#4367=ORIENTED_EDGE('',*,*,#3358,.T.);
#4368=ORIENTED_EDGE('',*,*,#3344,.T.);
#4369=ORIENTED_EDGE('',*,*,#3354,.F.);
#4370=ORIENTED_EDGE('',*,*,#3359,.F.);
#4371=ORIENTED_EDGE('',*,*,#3360,.F.);
#4372=ORIENTED_EDGE('',*,*,#3361,.F.);
#4373=ORIENTED_EDGE('',*,*,#3362,.F.);
#4374=ORIENTED_EDGE('',*,*,#3363,.T.);
#4375=ORIENTED_EDGE('',*,*,#3357,.F.);
#4376=ORIENTED_EDGE('',*,*,#3364,.F.);
#4377=ORIENTED_EDGE('',*,*,#3365,.F.);
#4378=ORIENTED_EDGE('',*,*,#3366,.F.);
#4379=ORIENTED_EDGE('',*,*,#3359,.T.);
#4380=ORIENTED_EDGE('',*,*,#3343,.F.);
#4381=ORIENTED_EDGE('',*,*,#3367,.F.);
#4382=ORIENTED_EDGE('',*,*,#3368,.F.);
#4383=ORIENTED_EDGE('',*,*,#3364,.T.);
#4384=ORIENTED_EDGE('',*,*,#3369,.F.);
#4385=ORIENTED_EDGE('',*,*,#3370,.F.);
#4386=ORIENTED_EDGE('',*,*,#3371,.F.);
#4387=ORIENTED_EDGE('',*,*,#3372,.F.);
#4388=ORIENTED_EDGE('',*,*,#3373,.F.);
#4389=ORIENTED_EDGE('',*,*,#3374,.F.);
#4390=ORIENTED_EDGE('',*,*,#3375,.F.);
#4391=ORIENTED_EDGE('',*,*,#3376,.F.);
#4392=ORIENTED_EDGE('',*,*,#3377,.F.);
#4393=ORIENTED_EDGE('',*,*,#3341,.F.);
#4394=ORIENTED_EDGE('',*,*,#3358,.F.);
#4395=ORIENTED_EDGE('',*,*,#3355,.F.);
#4396=ORIENTED_EDGE('',*,*,#3351,.F.);
#4397=ORIENTED_EDGE('',*,*,#3348,.F.);
#4398=ORIENTED_EDGE('',*,*,#3345,.F.);
#4399=ORIENTED_EDGE('',*,*,#3378,.T.);
#4400=ORIENTED_EDGE('',*,*,#3379,.T.);
#4401=ORIENTED_EDGE('',*,*,#3369,.T.);
#4402=ORIENTED_EDGE('',*,*,#3380,.T.);
#4403=ORIENTED_EDGE('',*,*,#3381,.T.);
#4404=ORIENTED_EDGE('',*,*,#3382,.F.);
#4405=ORIENTED_EDGE('',*,*,#3371,.T.);
#4406=ORIENTED_EDGE('',*,*,#3377,.T.);
#4407=ORIENTED_EDGE('',*,*,#3383,.T.);
#4408=ORIENTED_EDGE('',*,*,#3384,.T.);
#4409=ORIENTED_EDGE('',*,*,#3380,.F.);
#4410=ORIENTED_EDGE('',*,*,#3385,.T.);
#4411=ORIENTED_EDGE('',*,*,#3373,.T.);
#4412=ORIENTED_EDGE('',*,*,#3386,.T.);
#4413=ORIENTED_EDGE('',*,*,#3387,.T.);
#4414=ORIENTED_EDGE('',*,*,#3383,.F.);
#4415=ORIENTED_EDGE('',*,*,#3376,.T.);
#4416=ORIENTED_EDGE('',*,*,#3388,.T.);
#4417=ORIENTED_EDGE('',*,*,#3386,.F.);
#4418=ORIENTED_EDGE('',*,*,#3372,.T.);
#4419=ORIENTED_EDGE('',*,*,#3382,.T.);
#4420=ORIENTED_EDGE('',*,*,#3388,.F.);
#4421=ORIENTED_EDGE('',*,*,#3389,.F.);
#4422=ORIENTED_EDGE('',*,*,#3390,.T.);
#4423=ORIENTED_EDGE('',*,*,#3391,.T.);
#4424=ORIENTED_EDGE('',*,*,#3381,.F.);
#4425=ORIENTED_EDGE('',*,*,#3392,.F.);
#4426=ORIENTED_EDGE('',*,*,#3393,.T.);
#4427=ORIENTED_EDGE('',*,*,#3389,.T.);
#4428=ORIENTED_EDGE('',*,*,#3378,.F.);
#4429=ORIENTED_EDGE('',*,*,#3370,.T.);
#4430=ORIENTED_EDGE('',*,*,#3379,.F.);
#4431=ORIENTED_EDGE('',*,*,#3394,.T.);
#4432=ORIENTED_EDGE('',*,*,#3395,.T.);
#4433=ORIENTED_EDGE('',*,*,#3396,.T.);
#4434=ORIENTED_EDGE('',*,*,#3394,.F.);
#4435=ORIENTED_EDGE('',*,*,#3385,.F.);
#4436=ORIENTED_EDGE('',*,*,#3375,.T.);
#4437=ORIENTED_EDGE('',*,*,#3397,.T.);
#4438=ORIENTED_EDGE('',*,*,#3398,.T.);
#4439=ORIENTED_EDGE('',*,*,#3399,.T.);
#4440=ORIENTED_EDGE('',*,*,#3397,.F.);
#4441=ORIENTED_EDGE('',*,*,#3374,.T.);
#4442=ORIENTED_EDGE('',*,*,#3395,.F.);
#4443=ORIENTED_EDGE('',*,*,#3396,.F.);
#4444=ORIENTED_EDGE('',*,*,#3400,.T.);
#4445=ORIENTED_EDGE('',*,*,#3401,.F.);
#4446=ORIENTED_EDGE('',*,*,#3400,.F.);
#4447=ORIENTED_EDGE('',*,*,#3398,.F.);
#4448=ORIENTED_EDGE('',*,*,#3399,.F.);
#4449=ORIENTED_EDGE('',*,*,#3402,.T.);
#4450=ORIENTED_EDGE('',*,*,#3403,.F.);
#4451=ORIENTED_EDGE('',*,*,#3402,.F.);
#4452=ORIENTED_EDGE('',*,*,#3337,.T.);
#4453=ORIENTED_EDGE('',*,*,#3404,.T.);
#4454=ORIENTED_EDGE('',*,*,#3334,.F.);
#4455=ORIENTED_EDGE('',*,*,#3405,.F.);
#4456=ORIENTED_EDGE('',*,*,#3406,.F.);
#4457=ORIENTED_EDGE('',*,*,#3304,.F.);
#4458=ORIENTED_EDGE('',*,*,#3308,.F.);
#4459=ORIENTED_EDGE('',*,*,#3311,.F.);
#4460=ORIENTED_EDGE('',*,*,#3314,.F.);
#4461=ORIENTED_EDGE('',*,*,#3317,.F.);
#4462=ORIENTED_EDGE('',*,*,#3320,.F.);
#4463=ORIENTED_EDGE('',*,*,#3323,.F.);
#4464=ORIENTED_EDGE('',*,*,#3326,.F.);
#4465=ORIENTED_EDGE('',*,*,#3329,.F.);
#4466=ORIENTED_EDGE('',*,*,#3332,.F.);
#4467=ORIENTED_EDGE('',*,*,#3335,.F.);
#4468=ORIENTED_EDGE('',*,*,#3404,.F.);
#4469=ORIENTED_EDGE('',*,*,#3340,.F.);
#4470=ORIENTED_EDGE('',*,*,#3407,.F.);
#4471=ORIENTED_EDGE('',*,*,#3408,.F.);
#4472=ORIENTED_EDGE('',*,*,#3149,.F.);
#4473=ORIENTED_EDGE('',*,*,#3409,.F.);
#4474=ORIENTED_EDGE('',*,*,#3147,.F.);
#4475=ORIENTED_EDGE('',*,*,#3144,.F.);
#4476=ORIENTED_EDGE('',*,*,#3141,.F.);
#4477=ORIENTED_EDGE('',*,*,#3138,.F.);
#4478=ORIENTED_EDGE('',*,*,#3135,.F.);
#4479=ORIENTED_EDGE('',*,*,#3132,.F.);
#4480=ORIENTED_EDGE('',*,*,#3129,.F.);
#4481=ORIENTED_EDGE('',*,*,#3126,.F.);
#4482=ORIENTED_EDGE('',*,*,#3123,.F.);
#4483=ORIENTED_EDGE('',*,*,#3120,.F.);
#4484=ORIENTED_EDGE('',*,*,#3410,.F.);
#4485=ORIENTED_EDGE('',*,*,#3118,.F.);
#4486=ORIENTED_EDGE('',*,*,#3122,.F.);
#4487=ORIENTED_EDGE('',*,*,#3125,.F.);
#4488=ORIENTED_EDGE('',*,*,#3128,.F.);
#4489=ORIENTED_EDGE('',*,*,#3131,.F.);
#4490=ORIENTED_EDGE('',*,*,#3134,.F.);
#4491=ORIENTED_EDGE('',*,*,#3137,.F.);
#4492=ORIENTED_EDGE('',*,*,#3140,.F.);
#4493=ORIENTED_EDGE('',*,*,#3143,.F.);
#4494=ORIENTED_EDGE('',*,*,#3146,.F.);
#4495=ORIENTED_EDGE('',*,*,#3411,.F.);
#4496=ORIENTED_EDGE('',*,*,#3152,.F.);
#4497=ORIENTED_EDGE('',*,*,#3412,.F.);
#4498=ORIENTED_EDGE('',*,*,#3338,.T.);
#4499=ORIENTED_EDGE('',*,*,#3405,.T.);
#4500=ORIENTED_EDGE('',*,*,#3336,.T.);
#4501=ORIENTED_EDGE('',*,*,#3333,.T.);
#4502=ORIENTED_EDGE('',*,*,#3330,.T.);
#4503=ORIENTED_EDGE('',*,*,#3327,.T.);
#4504=ORIENTED_EDGE('',*,*,#3324,.T.);
#4505=ORIENTED_EDGE('',*,*,#3321,.T.);
#4506=ORIENTED_EDGE('',*,*,#3318,.T.);
#4507=ORIENTED_EDGE('',*,*,#3315,.T.);
#4508=ORIENTED_EDGE('',*,*,#3312,.T.);
#4509=ORIENTED_EDGE('',*,*,#3309,.T.);
#4510=ORIENTED_EDGE('',*,*,#3306,.T.);
#4511=ORIENTED_EDGE('',*,*,#3413,.F.);
#4512=ORIENTED_EDGE('',*,*,#3414,.F.);
#4513=ORIENTED_EDGE('',*,*,#3415,.F.);
#4514=ORIENTED_EDGE('',*,*,#3416,.F.);
#4515=ORIENTED_EDGE('',*,*,#3417,.F.);
#4516=ORIENTED_EDGE('',*,*,#3418,.F.);
#4517=ORIENTED_EDGE('',*,*,#3410,.T.);
#4518=ORIENTED_EDGE('',*,*,#3305,.T.);
#4519=ORIENTED_EDGE('',*,*,#3406,.T.);
#4520=ORIENTED_EDGE('',*,*,#3119,.T.);
#4521=ORIENTED_EDGE('',*,*,#3419,.T.);
#4522=ORIENTED_EDGE('',*,*,#3420,.T.);
#4523=ORIENTED_EDGE('',*,*,#3421,.T.);
#4524=ORIENTED_EDGE('',*,*,#3422,.T.);
#4525=ORIENTED_EDGE('',*,*,#3423,.T.);
#4526=ORIENTED_EDGE('',*,*,#3424,.T.);
#4527=ORIENTED_EDGE('',*,*,#3425,.T.);
#4528=ORIENTED_EDGE('',*,*,#3426,.T.);
#4529=ORIENTED_EDGE('',*,*,#3427,.T.);
#4530=ORIENTED_EDGE('',*,*,#3428,.T.);
#4531=ORIENTED_EDGE('',*,*,#3429,.T.);
#4532=ORIENTED_EDGE('',*,*,#3430,.T.);
#4533=ORIENTED_EDGE('',*,*,#3431,.T.);
#4534=ORIENTED_EDGE('',*,*,#3155,.T.);
#4535=ORIENTED_EDGE('',*,*,#3432,.T.);
#4536=ORIENTED_EDGE('',*,*,#3191,.T.);
#4537=ORIENTED_EDGE('',*,*,#3433,.T.);
#4538=ORIENTED_EDGE('',*,*,#3084,.T.);
#4539=ORIENTED_EDGE('',*,*,#3434,.T.);
#4540=ORIENTED_EDGE('',*,*,#3229,.T.);
#4541=ORIENTED_EDGE('',*,*,#3435,.T.);
#4542=ORIENTED_EDGE('',*,*,#3049,.T.);
#4543=ORIENTED_EDGE('',*,*,#3436,.T.);
#4544=ORIENTED_EDGE('',*,*,#3267,.T.);
#4545=ORIENTED_EDGE('',*,*,#3299,.T.);
#4546=ORIENTED_EDGE('',*,*,#3437,.T.);
#4547=ORIENTED_EDGE('',*,*,#3296,.F.);
#4548=ORIENTED_EDGE('',*,*,#3438,.F.);
#4549=ORIENTED_EDGE('',*,*,#3435,.F.);
#4550=ORIENTED_EDGE('',*,*,#3266,.F.);
#4551=ORIENTED_EDGE('',*,*,#3270,.F.);
#4552=ORIENTED_EDGE('',*,*,#3273,.F.);
#4553=ORIENTED_EDGE('',*,*,#3276,.F.);
#4554=ORIENTED_EDGE('',*,*,#3279,.F.);
#4555=ORIENTED_EDGE('',*,*,#3282,.F.);
#4556=ORIENTED_EDGE('',*,*,#3285,.F.);
#4557=ORIENTED_EDGE('',*,*,#3288,.F.);
#4558=ORIENTED_EDGE('',*,*,#3291,.F.);
#4559=ORIENTED_EDGE('',*,*,#3294,.F.);
#4560=ORIENTED_EDGE('',*,*,#3297,.F.);
#4561=ORIENTED_EDGE('',*,*,#3437,.F.);
#4562=ORIENTED_EDGE('',*,*,#3302,.F.);
#4563=ORIENTED_EDGE('',*,*,#3439,.F.);
#4564=ORIENTED_EDGE('',*,*,#3079,.F.);
#4565=ORIENTED_EDGE('',*,*,#3440,.F.);
#4566=ORIENTED_EDGE('',*,*,#3077,.F.);
#4567=ORIENTED_EDGE('',*,*,#3074,.F.);
#4568=ORIENTED_EDGE('',*,*,#3071,.F.);
#4569=ORIENTED_EDGE('',*,*,#3068,.F.);
#4570=ORIENTED_EDGE('',*,*,#3065,.F.);
#4571=ORIENTED_EDGE('',*,*,#3062,.F.);
#4572=ORIENTED_EDGE('',*,*,#3059,.F.);
#4573=ORIENTED_EDGE('',*,*,#3056,.F.);
#4574=ORIENTED_EDGE('',*,*,#3053,.F.);
#4575=ORIENTED_EDGE('',*,*,#3050,.F.);
#4576=ORIENTED_EDGE('',*,*,#3436,.F.);
#4577=ORIENTED_EDGE('',*,*,#3048,.F.);
#4578=ORIENTED_EDGE('',*,*,#3052,.F.);
#4579=ORIENTED_EDGE('',*,*,#3055,.F.);
#4580=ORIENTED_EDGE('',*,*,#3058,.F.);
#4581=ORIENTED_EDGE('',*,*,#3061,.F.);
#4582=ORIENTED_EDGE('',*,*,#3064,.F.);
#4583=ORIENTED_EDGE('',*,*,#3067,.F.);
#4584=ORIENTED_EDGE('',*,*,#3070,.F.);
#4585=ORIENTED_EDGE('',*,*,#3073,.F.);
#4586=ORIENTED_EDGE('',*,*,#3076,.F.);
#4587=ORIENTED_EDGE('',*,*,#3441,.F.);
#4588=ORIENTED_EDGE('',*,*,#3081,.F.);
#4589=ORIENTED_EDGE('',*,*,#3442,.F.);
#4590=ORIENTED_EDGE('',*,*,#3300,.T.);
#4591=ORIENTED_EDGE('',*,*,#3438,.T.);
#4592=ORIENTED_EDGE('',*,*,#3298,.T.);
#4593=ORIENTED_EDGE('',*,*,#3295,.T.);
#4594=ORIENTED_EDGE('',*,*,#3292,.T.);
#4595=ORIENTED_EDGE('',*,*,#3289,.T.);
#4596=ORIENTED_EDGE('',*,*,#3286,.T.);
#4597=ORIENTED_EDGE('',*,*,#3283,.T.);
#4598=ORIENTED_EDGE('',*,*,#3280,.T.);
#4599=ORIENTED_EDGE('',*,*,#3277,.T.);
#4600=ORIENTED_EDGE('',*,*,#3274,.T.);
#4601=ORIENTED_EDGE('',*,*,#3271,.T.);
#4602=ORIENTED_EDGE('',*,*,#3268,.T.);
#4603=ORIENTED_EDGE('',*,*,#3261,.T.);
#4604=ORIENTED_EDGE('',*,*,#3443,.T.);
#4605=ORIENTED_EDGE('',*,*,#3258,.F.);
#4606=ORIENTED_EDGE('',*,*,#3444,.F.);
#4607=ORIENTED_EDGE('',*,*,#3433,.F.);
#4608=ORIENTED_EDGE('',*,*,#3228,.F.);
#4609=ORIENTED_EDGE('',*,*,#3232,.F.);
#4610=ORIENTED_EDGE('',*,*,#3235,.F.);
#4611=ORIENTED_EDGE('',*,*,#3238,.F.);
#4612=ORIENTED_EDGE('',*,*,#3241,.F.);
#4613=ORIENTED_EDGE('',*,*,#3244,.F.);
#4614=ORIENTED_EDGE('',*,*,#3247,.F.);
#4615=ORIENTED_EDGE('',*,*,#3250,.F.);
#4616=ORIENTED_EDGE('',*,*,#3253,.F.);
#4617=ORIENTED_EDGE('',*,*,#3256,.F.);
#4618=ORIENTED_EDGE('',*,*,#3259,.F.);
#4619=ORIENTED_EDGE('',*,*,#3443,.F.);
#4620=ORIENTED_EDGE('',*,*,#3264,.F.);
#4621=ORIENTED_EDGE('',*,*,#3445,.F.);
#4622=ORIENTED_EDGE('',*,*,#3114,.F.);
#4623=ORIENTED_EDGE('',*,*,#3446,.F.);
#4624=ORIENTED_EDGE('',*,*,#3112,.F.);
#4625=ORIENTED_EDGE('',*,*,#3109,.F.);
#4626=ORIENTED_EDGE('',*,*,#3106,.F.);
#4627=ORIENTED_EDGE('',*,*,#3103,.F.);
#4628=ORIENTED_EDGE('',*,*,#3100,.F.);
#4629=ORIENTED_EDGE('',*,*,#3097,.F.);
#4630=ORIENTED_EDGE('',*,*,#3094,.F.);
#4631=ORIENTED_EDGE('',*,*,#3091,.F.);
#4632=ORIENTED_EDGE('',*,*,#3088,.F.);
#4633=ORIENTED_EDGE('',*,*,#3085,.F.);
#4634=ORIENTED_EDGE('',*,*,#3434,.F.);
#4635=ORIENTED_EDGE('',*,*,#3083,.F.);
#4636=ORIENTED_EDGE('',*,*,#3087,.F.);
#4637=ORIENTED_EDGE('',*,*,#3090,.F.);
#4638=ORIENTED_EDGE('',*,*,#3093,.F.);
#4639=ORIENTED_EDGE('',*,*,#3096,.F.);
#4640=ORIENTED_EDGE('',*,*,#3099,.F.);
#4641=ORIENTED_EDGE('',*,*,#3102,.F.);
#4642=ORIENTED_EDGE('',*,*,#3105,.F.);
#4643=ORIENTED_EDGE('',*,*,#3108,.F.);
#4644=ORIENTED_EDGE('',*,*,#3111,.F.);
#4645=ORIENTED_EDGE('',*,*,#3447,.F.);
#4646=ORIENTED_EDGE('',*,*,#3116,.F.);
#4647=ORIENTED_EDGE('',*,*,#3448,.F.);
#4648=ORIENTED_EDGE('',*,*,#3262,.T.);
#4649=ORIENTED_EDGE('',*,*,#3444,.T.);
#4650=ORIENTED_EDGE('',*,*,#3260,.T.);
#4651=ORIENTED_EDGE('',*,*,#3257,.T.);
#4652=ORIENTED_EDGE('',*,*,#3254,.T.);
#4653=ORIENTED_EDGE('',*,*,#3251,.T.);
#4654=ORIENTED_EDGE('',*,*,#3248,.T.);
#4655=ORIENTED_EDGE('',*,*,#3245,.T.);
#4656=ORIENTED_EDGE('',*,*,#3242,.T.);
#4657=ORIENTED_EDGE('',*,*,#3239,.T.);
#4658=ORIENTED_EDGE('',*,*,#3236,.T.);
#4659=ORIENTED_EDGE('',*,*,#3233,.T.);
#4660=ORIENTED_EDGE('',*,*,#3230,.T.);
#4661=ORIENTED_EDGE('',*,*,#3223,.T.);
#4662=ORIENTED_EDGE('',*,*,#3449,.T.);
#4663=ORIENTED_EDGE('',*,*,#3220,.F.);
#4664=ORIENTED_EDGE('',*,*,#3450,.F.);
#4665=ORIENTED_EDGE('',*,*,#3431,.F.);
#4666=ORIENTED_EDGE('',*,*,#3190,.F.);
#4667=ORIENTED_EDGE('',*,*,#3194,.F.);
#4668=ORIENTED_EDGE('',*,*,#3197,.F.);
#4669=ORIENTED_EDGE('',*,*,#3200,.F.);
#4670=ORIENTED_EDGE('',*,*,#3203,.F.);
#4671=ORIENTED_EDGE('',*,*,#3206,.F.);
#4672=ORIENTED_EDGE('',*,*,#3209,.F.);
#4673=ORIENTED_EDGE('',*,*,#3212,.F.);
#4674=ORIENTED_EDGE('',*,*,#3215,.F.);
#4675=ORIENTED_EDGE('',*,*,#3218,.F.);
#4676=ORIENTED_EDGE('',*,*,#3221,.F.);
#4677=ORIENTED_EDGE('',*,*,#3449,.F.);
#4678=ORIENTED_EDGE('',*,*,#3226,.F.);
#4679=ORIENTED_EDGE('',*,*,#3451,.F.);
#4680=ORIENTED_EDGE('',*,*,#3185,.F.);
#4681=ORIENTED_EDGE('',*,*,#3452,.F.);
#4682=ORIENTED_EDGE('',*,*,#3183,.F.);
#4683=ORIENTED_EDGE('',*,*,#3180,.F.);
#4684=ORIENTED_EDGE('',*,*,#3177,.F.);
#4685=ORIENTED_EDGE('',*,*,#3174,.F.);
#4686=ORIENTED_EDGE('',*,*,#3171,.F.);
#4687=ORIENTED_EDGE('',*,*,#3168,.F.);
#4688=ORIENTED_EDGE('',*,*,#3165,.F.);
#4689=ORIENTED_EDGE('',*,*,#3162,.F.);
#4690=ORIENTED_EDGE('',*,*,#3159,.F.);
#4691=ORIENTED_EDGE('',*,*,#3156,.F.);
#4692=ORIENTED_EDGE('',*,*,#3432,.F.);
#4693=ORIENTED_EDGE('',*,*,#3154,.F.);
#4694=ORIENTED_EDGE('',*,*,#3158,.F.);
#4695=ORIENTED_EDGE('',*,*,#3161,.F.);
#4696=ORIENTED_EDGE('',*,*,#3164,.F.);
#4697=ORIENTED_EDGE('',*,*,#3167,.F.);
#4698=ORIENTED_EDGE('',*,*,#3170,.F.);
#4699=ORIENTED_EDGE('',*,*,#3173,.F.);
#4700=ORIENTED_EDGE('',*,*,#3176,.F.);
#4701=ORIENTED_EDGE('',*,*,#3179,.F.);
#4702=ORIENTED_EDGE('',*,*,#3182,.F.);
#4703=ORIENTED_EDGE('',*,*,#3453,.F.);
#4704=ORIENTED_EDGE('',*,*,#3188,.F.);
#4705=ORIENTED_EDGE('',*,*,#3454,.F.);
#4706=ORIENTED_EDGE('',*,*,#3455,.F.);
#4707=ORIENTED_EDGE('',*,*,#3224,.T.);
#4708=ORIENTED_EDGE('',*,*,#3450,.T.);
#4709=ORIENTED_EDGE('',*,*,#3222,.T.);
#4710=ORIENTED_EDGE('',*,*,#3219,.T.);
#4711=ORIENTED_EDGE('',*,*,#3216,.T.);
#4712=ORIENTED_EDGE('',*,*,#3213,.T.);
#4713=ORIENTED_EDGE('',*,*,#3210,.T.);
#4714=ORIENTED_EDGE('',*,*,#3207,.T.);
#4715=ORIENTED_EDGE('',*,*,#3204,.T.);
#4716=ORIENTED_EDGE('',*,*,#3201,.T.);
#4717=ORIENTED_EDGE('',*,*,#3198,.T.);
#4718=ORIENTED_EDGE('',*,*,#3195,.T.);
#4719=ORIENTED_EDGE('',*,*,#3192,.T.);
#4720=ORIENTED_EDGE('',*,*,#3408,.T.);
#4721=ORIENTED_EDGE('',*,*,#3361,.T.);
#4722=ORIENTED_EDGE('',*,*,#3454,.T.);
#4723=ORIENTED_EDGE('',*,*,#3187,.T.);
#4724=ORIENTED_EDGE('',*,*,#3365,.T.);
#4725=ORIENTED_EDGE('',*,*,#3368,.T.);
#4726=ORIENTED_EDGE('',*,*,#3456,.T.);
#4727=ORIENTED_EDGE('',*,*,#3457,.T.);
#4728=ORIENTED_EDGE('',*,*,#3458,.T.);
#4729=ORIENTED_EDGE('',*,*,#3150,.T.);
#4730=ORIENTED_EDGE('',*,*,#3459,.T.);
#4731=ORIENTED_EDGE('',*,*,#3460,.T.);
#4732=ORIENTED_EDGE('',*,*,#3461,.T.);
#4733=ORIENTED_EDGE('',*,*,#3462,.T.);
#4734=ORIENTED_EDGE('',*,*,#3463,.T.);
#4735=ORIENTED_EDGE('',*,*,#3464,.T.);
#4736=ORIENTED_EDGE('',*,*,#3465,.T.);
#4737=ORIENTED_EDGE('',*,*,#3466,.T.);
#4738=ORIENTED_EDGE('',*,*,#3467,.T.);
#4739=ORIENTED_EDGE('',*,*,#3468,.T.);
#4740=ORIENTED_EDGE('',*,*,#3469,.T.);
#4741=ORIENTED_EDGE('',*,*,#3470,.T.);
#4742=ORIENTED_EDGE('',*,*,#3366,.T.);
#4743=ORIENTED_EDGE('',*,*,#3186,.F.);
#4744=ORIENTED_EDGE('',*,*,#3451,.T.);
#4745=ORIENTED_EDGE('',*,*,#3225,.T.);
#4746=ORIENTED_EDGE('',*,*,#3455,.T.);
#4747=ORIENTED_EDGE('',*,*,#3360,.T.);
#4748=ORIENTED_EDGE('',*,*,#3184,.T.);
#4749=ORIENTED_EDGE('',*,*,#3453,.T.);
#4750=ORIENTED_EDGE('',*,*,#3181,.F.);
#4751=ORIENTED_EDGE('',*,*,#3452,.T.);
#4752=ORIENTED_EDGE('',*,*,#3362,.T.);
#4753=ORIENTED_EDGE('',*,*,#3407,.T.);
#4754=ORIENTED_EDGE('',*,*,#3339,.T.);
#4755=ORIENTED_EDGE('',*,*,#3412,.T.);
#4756=ORIENTED_EDGE('',*,*,#3151,.F.);
#4757=ORIENTED_EDGE('',*,*,#3471,.T.);
#4758=ORIENTED_EDGE('',*,*,#3148,.T.);
#4759=ORIENTED_EDGE('',*,*,#3411,.T.);
#4760=ORIENTED_EDGE('',*,*,#3145,.F.);
#4761=ORIENTED_EDGE('',*,*,#3409,.T.);
#4762=ORIENTED_EDGE('',*,*,#3113,.T.);
#4763=ORIENTED_EDGE('',*,*,#3447,.T.);
#4764=ORIENTED_EDGE('',*,*,#3110,.F.);
#4765=ORIENTED_EDGE('',*,*,#3446,.T.);
#4766=ORIENTED_EDGE('',*,*,#3445,.T.);
#4767=ORIENTED_EDGE('',*,*,#3263,.T.);
#4768=ORIENTED_EDGE('',*,*,#3448,.T.);
#4769=ORIENTED_EDGE('',*,*,#3115,.F.);
#4770=ORIENTED_EDGE('',*,*,#3078,.T.);
#4771=ORIENTED_EDGE('',*,*,#3441,.T.);
#4772=ORIENTED_EDGE('',*,*,#3075,.F.);
#4773=ORIENTED_EDGE('',*,*,#3440,.T.);
#4774=ORIENTED_EDGE('',*,*,#3439,.T.);
#4775=ORIENTED_EDGE('',*,*,#3301,.T.);
#4776=ORIENTED_EDGE('',*,*,#3442,.T.);
#4777=ORIENTED_EDGE('',*,*,#3080,.F.);
#4778=ORIENTED_EDGE('',*,*,#3467,.F.);
#4779=ORIENTED_EDGE('',*,*,#3472,.T.);
#4780=ORIENTED_EDGE('',*,*,#3419,.F.);
#4781=ORIENTED_EDGE('',*,*,#3473,.F.);
#4782=ORIENTED_EDGE('',*,*,#3470,.F.);
#4783=ORIENTED_EDGE('',*,*,#3474,.T.);
#4784=ORIENTED_EDGE('',*,*,#3420,.F.);
#4785=ORIENTED_EDGE('',*,*,#3472,.F.);
#4786=ORIENTED_EDGE('',*,*,#3469,.F.);
#4787=ORIENTED_EDGE('',*,*,#3475,.T.);
#4788=ORIENTED_EDGE('',*,*,#3421,.F.);
#4789=ORIENTED_EDGE('',*,*,#3474,.F.);
#4790=ORIENTED_EDGE('',*,*,#3468,.F.);
#4791=ORIENTED_EDGE('',*,*,#3473,.T.);
#4792=ORIENTED_EDGE('',*,*,#3422,.F.);
#4793=ORIENTED_EDGE('',*,*,#3475,.F.);
#4794=ORIENTED_EDGE('',*,*,#3463,.F.);
#4795=ORIENTED_EDGE('',*,*,#3476,.T.);
#4796=ORIENTED_EDGE('',*,*,#3423,.F.);
#4797=ORIENTED_EDGE('',*,*,#3477,.F.);
#4798=ORIENTED_EDGE('',*,*,#3466,.F.);
#4799=ORIENTED_EDGE('',*,*,#3478,.T.);
#4800=ORIENTED_EDGE('',*,*,#3424,.F.);
#4801=ORIENTED_EDGE('',*,*,#3476,.F.);
#4802=ORIENTED_EDGE('',*,*,#3465,.F.);
#4803=ORIENTED_EDGE('',*,*,#3479,.T.);
#4804=ORIENTED_EDGE('',*,*,#3425,.F.);
#4805=ORIENTED_EDGE('',*,*,#3478,.F.);
#4806=ORIENTED_EDGE('',*,*,#3464,.F.);
#4807=ORIENTED_EDGE('',*,*,#3477,.T.);
#4808=ORIENTED_EDGE('',*,*,#3426,.F.);
#4809=ORIENTED_EDGE('',*,*,#3479,.F.);
#4810=ORIENTED_EDGE('',*,*,#3459,.F.);
#4811=ORIENTED_EDGE('',*,*,#3480,.T.);
#4812=ORIENTED_EDGE('',*,*,#3427,.F.);
#4813=ORIENTED_EDGE('',*,*,#3481,.F.);
#4814=ORIENTED_EDGE('',*,*,#3462,.F.);
#4815=ORIENTED_EDGE('',*,*,#3482,.T.);
#4816=ORIENTED_EDGE('',*,*,#3428,.F.);
#4817=ORIENTED_EDGE('',*,*,#3480,.F.);
#4818=ORIENTED_EDGE('',*,*,#3461,.F.);
#4819=ORIENTED_EDGE('',*,*,#3483,.T.);
#4820=ORIENTED_EDGE('',*,*,#3429,.F.);
#4821=ORIENTED_EDGE('',*,*,#3482,.F.);
#4822=ORIENTED_EDGE('',*,*,#3460,.F.);
#4823=ORIENTED_EDGE('',*,*,#3481,.T.);
#4824=ORIENTED_EDGE('',*,*,#3430,.F.);
#4825=ORIENTED_EDGE('',*,*,#3483,.F.);
#4826=ORIENTED_EDGE('',*,*,#3484,.F.);
#4827=ORIENTED_EDGE('',*,*,#3390,.F.);
#4828=ORIENTED_EDGE('',*,*,#3393,.F.);
#4829=ORIENTED_EDGE('',*,*,#3485,.F.);
#4830=ORIENTED_EDGE('',*,*,#3403,.T.);
#4831=ORIENTED_EDGE('',*,*,#3401,.T.);
#4832=ORIENTED_EDGE('',*,*,#3486,.F.);
#4833=ORIENTED_EDGE('',*,*,#3487,.F.);
#4834=ORIENTED_EDGE('',*,*,#3488,.F.);
#4835=ORIENTED_EDGE('',*,*,#3489,.F.);
#4836=ORIENTED_EDGE('',*,*,#3490,.F.);
#4837=ORIENTED_EDGE('',*,*,#3491,.F.);
#4838=ORIENTED_EDGE('',*,*,#3384,.F.);
#4839=ORIENTED_EDGE('',*,*,#3492,.F.);
#4840=ORIENTED_EDGE('',*,*,#3485,.T.);
#4841=ORIENTED_EDGE('',*,*,#3392,.T.);
#4842=ORIENTED_EDGE('',*,*,#3387,.F.);
#4843=ORIENTED_EDGE('',*,*,#3391,.F.);
#4844=ORIENTED_EDGE('',*,*,#3484,.T.);
#4845=ORIENTED_EDGE('',*,*,#3492,.T.);
#4846=ORIENTED_EDGE('',*,*,#3347,.F.);
#4847=ORIENTED_EDGE('',*,*,#3493,.F.);
#4848=ORIENTED_EDGE('',*,*,#3456,.F.);
#4849=ORIENTED_EDGE('',*,*,#3367,.T.);
#4850=ORIENTED_EDGE('',*,*,#3350,.F.);
#4851=ORIENTED_EDGE('',*,*,#3494,.F.);
#4852=ORIENTED_EDGE('',*,*,#3457,.F.);
#4853=ORIENTED_EDGE('',*,*,#3493,.T.);
#4854=ORIENTED_EDGE('',*,*,#3489,.T.);
#4855=ORIENTED_EDGE('',*,*,#3495,.F.);
#4856=ORIENTED_EDGE('',*,*,#3417,.T.);
#4857=ORIENTED_EDGE('',*,*,#3496,.T.);
#4858=ORIENTED_EDGE('',*,*,#3488,.T.);
#4859=ORIENTED_EDGE('',*,*,#3497,.F.);
#4860=ORIENTED_EDGE('',*,*,#3418,.T.);
#4861=ORIENTED_EDGE('',*,*,#3495,.T.);
#4862=ORIENTED_EDGE('',*,*,#3487,.T.);
#4863=ORIENTED_EDGE('',*,*,#3498,.F.);
#4864=ORIENTED_EDGE('',*,*,#3413,.T.);
#4865=ORIENTED_EDGE('',*,*,#3497,.T.);
#4866=ORIENTED_EDGE('',*,*,#3353,.F.);
#4867=ORIENTED_EDGE('',*,*,#3363,.F.);
#4868=ORIENTED_EDGE('',*,*,#3471,.F.);
#4869=ORIENTED_EDGE('',*,*,#3458,.F.);
#4870=ORIENTED_EDGE('',*,*,#3494,.T.);
#4871=ORIENTED_EDGE('',*,*,#3486,.T.);
#4872=ORIENTED_EDGE('',*,*,#3499,.F.);
#4873=ORIENTED_EDGE('',*,*,#3414,.T.);
#4874=ORIENTED_EDGE('',*,*,#3498,.T.);
#4875=ORIENTED_EDGE('',*,*,#3491,.T.);
#4876=ORIENTED_EDGE('',*,*,#3500,.F.);
#4877=ORIENTED_EDGE('',*,*,#3415,.T.);
#4878=ORIENTED_EDGE('',*,*,#3499,.T.);
#4879=ORIENTED_EDGE('',*,*,#3490,.T.);
#4880=ORIENTED_EDGE('',*,*,#3496,.F.);
#4881=ORIENTED_EDGE('',*,*,#3416,.T.);
#4882=ORIENTED_EDGE('',*,*,#3500,.T.);
#4883=ORIENTED_EDGE('',*,*,#3501,.F.);
#4884=ORIENTED_EDGE('',*,*,#3502,.F.);
#4885=ORIENTED_EDGE('',*,*,#3503,.F.);
#4886=ORIENTED_EDGE('',*,*,#3504,.F.);
#4887=ORIENTED_EDGE('',*,*,#3505,.F.);
#4888=ORIENTED_EDGE('',*,*,#3506,.F.);
#4889=ORIENTED_EDGE('',*,*,#3507,.F.);
#4890=ORIENTED_EDGE('',*,*,#3508,.F.);
#4891=ORIENTED_EDGE('',*,*,#3509,.F.);
#4892=ORIENTED_EDGE('',*,*,#3510,.F.);
#4893=ORIENTED_EDGE('',*,*,#3511,.F.);
#4894=ORIENTED_EDGE('',*,*,#3512,.F.);
#4895=ORIENTED_EDGE('',*,*,#3513,.F.);
#4896=ORIENTED_EDGE('',*,*,#3514,.F.);
#4897=ORIENTED_EDGE('',*,*,#3515,.F.);
#4898=ORIENTED_EDGE('',*,*,#3516,.F.);
#4899=ORIENTED_EDGE('',*,*,#3517,.F.);
#4900=ORIENTED_EDGE('',*,*,#3518,.F.);
#4901=ORIENTED_EDGE('',*,*,#3519,.F.);
#4902=ORIENTED_EDGE('',*,*,#3520,.F.);
#4903=ORIENTED_EDGE('',*,*,#3521,.F.);
#4904=ORIENTED_EDGE('',*,*,#3522,.F.);
#4905=ORIENTED_EDGE('',*,*,#3523,.F.);
#4906=ORIENTED_EDGE('',*,*,#3524,.F.);
#4907=ORIENTED_EDGE('',*,*,#3523,.T.);
#4908=ORIENTED_EDGE('',*,*,#3525,.T.);
#4909=ORIENTED_EDGE('',*,*,#3514,.T.);
#4910=ORIENTED_EDGE('',*,*,#3526,.T.);
#4911=ORIENTED_EDGE('',*,*,#3520,.T.);
#4912=ORIENTED_EDGE('',*,*,#3527,.T.);
#4913=ORIENTED_EDGE('',*,*,#3524,.T.);
#4914=ORIENTED_EDGE('',*,*,#3528,.T.);
#4915=ORIENTED_EDGE('',*,*,#3517,.T.);
#4916=ORIENTED_EDGE('',*,*,#3529,.T.);
#4917=ORIENTED_EDGE('',*,*,#3522,.T.);
#4918=ORIENTED_EDGE('',*,*,#3530,.T.);
#4919=ORIENTED_EDGE('',*,*,#3508,.T.);
#4920=ORIENTED_EDGE('',*,*,#3531,.T.);
#4921=ORIENTED_EDGE('',*,*,#3521,.T.);
#4922=ORIENTED_EDGE('',*,*,#3532,.T.);
#4923=ORIENTED_EDGE('',*,*,#3511,.T.);
#4924=ORIENTED_EDGE('',*,*,#3533,.T.);
#4925=ORIENTED_EDGE('',*,*,#3519,.T.);
#4926=ORIENTED_EDGE('',*,*,#3534,.T.);
#4927=ORIENTED_EDGE('',*,*,#3510,.T.);
#4928=ORIENTED_EDGE('',*,*,#3535,.T.);
#4929=ORIENTED_EDGE('',*,*,#3518,.T.);
#4930=ORIENTED_EDGE('',*,*,#3536,.T.);
#4931=ORIENTED_EDGE('',*,*,#3516,.T.);
#4932=ORIENTED_EDGE('',*,*,#3537,.T.);
#4933=ORIENTED_EDGE('',*,*,#3506,.T.);
#4934=ORIENTED_EDGE('',*,*,#3538,.T.);
#4935=ORIENTED_EDGE('',*,*,#3505,.T.);
#4936=ORIENTED_EDGE('',*,*,#3539,.T.);
#4937=ORIENTED_EDGE('',*,*,#3515,.T.);
#4938=ORIENTED_EDGE('',*,*,#3540,.T.);
#4939=ORIENTED_EDGE('',*,*,#3513,.T.);
#4940=ORIENTED_EDGE('',*,*,#3541,.T.);
#4941=ORIENTED_EDGE('',*,*,#3509,.T.);
#4942=ORIENTED_EDGE('',*,*,#3542,.T.);
#4943=ORIENTED_EDGE('',*,*,#3501,.T.);
#4944=ORIENTED_EDGE('',*,*,#3543,.T.);
#4945=ORIENTED_EDGE('',*,*,#3512,.T.);
#4946=ORIENTED_EDGE('',*,*,#3544,.T.);
#4947=ORIENTED_EDGE('',*,*,#3502,.T.);
#4948=ORIENTED_EDGE('',*,*,#3545,.T.);
#4949=ORIENTED_EDGE('',*,*,#3507,.T.);
#4950=ORIENTED_EDGE('',*,*,#3546,.T.);
#4951=ORIENTED_EDGE('',*,*,#3504,.T.);
#4952=ORIENTED_EDGE('',*,*,#3547,.T.);
#4953=ORIENTED_EDGE('',*,*,#3503,.T.);
#4954=ORIENTED_EDGE('',*,*,#3548,.T.);
#4955=ORIENTED_EDGE('',*,*,#3525,.F.);
#4956=ORIENTED_EDGE('',*,*,#3529,.F.);
#4957=ORIENTED_EDGE('',*,*,#3538,.F.);
#4958=ORIENTED_EDGE('',*,*,#3540,.F.);
#4959=ORIENTED_EDGE('',*,*,#3526,.F.);
#4960=ORIENTED_EDGE('',*,*,#3542,.F.);
#4961=ORIENTED_EDGE('',*,*,#3532,.F.);
#4962=ORIENTED_EDGE('',*,*,#3528,.F.);
#4963=ORIENTED_EDGE('',*,*,#3549,.T.);
#4964=ORIENTED_EDGE('',*,*,#3550,.T.);
#4965=ORIENTED_EDGE('',*,*,#3551,.T.);
#4966=ORIENTED_EDGE('',*,*,#3552,.T.);
#4967=ORIENTED_EDGE('',*,*,#3553,.T.);
#4968=ORIENTED_EDGE('',*,*,#3554,.T.);
#4969=ORIENTED_EDGE('',*,*,#3527,.F.);
#4970=ORIENTED_EDGE('',*,*,#3533,.F.);
#4971=ORIENTED_EDGE('',*,*,#3536,.F.);
#4972=ORIENTED_EDGE('',*,*,#3530,.F.);
#4973=ORIENTED_EDGE('',*,*,#3531,.F.);
#4974=ORIENTED_EDGE('',*,*,#3545,.F.);
#4975=ORIENTED_EDGE('',*,*,#3544,.F.);
#4976=ORIENTED_EDGE('',*,*,#3534,.F.);
#4977=ORIENTED_EDGE('',*,*,#3535,.F.);
#4978=ORIENTED_EDGE('',*,*,#3543,.F.);
#4979=ORIENTED_EDGE('',*,*,#3547,.F.);
#4980=ORIENTED_EDGE('',*,*,#3537,.F.);
#4981=ORIENTED_EDGE('',*,*,#3555,.T.);
#4982=ORIENTED_EDGE('',*,*,#3556,.T.);
#4983=ORIENTED_EDGE('',*,*,#3557,.T.);
#4984=ORIENTED_EDGE('',*,*,#3558,.T.);
#4985=ORIENTED_EDGE('',*,*,#3559,.T.);
#4986=ORIENTED_EDGE('',*,*,#3560,.T.);
#4987=ORIENTED_EDGE('',*,*,#3539,.F.);
#4988=ORIENTED_EDGE('',*,*,#3548,.F.);
#4989=ORIENTED_EDGE('',*,*,#3546,.F.);
#4990=ORIENTED_EDGE('',*,*,#3541,.F.);
#4991=ORIENTED_EDGE('',*,*,#3560,.F.);
#4992=ORIENTED_EDGE('',*,*,#3561,.T.);
#4993=ORIENTED_EDGE('',*,*,#3554,.F.);
#4994=ORIENTED_EDGE('',*,*,#3561,.F.);
#4995=ORIENTED_EDGE('',*,*,#3559,.F.);
#4996=ORIENTED_EDGE('',*,*,#3562,.T.);
#4997=ORIENTED_EDGE('',*,*,#3553,.F.);
#4998=ORIENTED_EDGE('',*,*,#3562,.F.);
#4999=ORIENTED_EDGE('',*,*,#3555,.F.);
#5000=ORIENTED_EDGE('',*,*,#3563,.T.);
#5001=ORIENTED_EDGE('',*,*,#3549,.F.);
#5002=ORIENTED_EDGE('',*,*,#3564,.F.);
#5003=ORIENTED_EDGE('',*,*,#3558,.F.);
#5004=ORIENTED_EDGE('',*,*,#3565,.T.);
#5005=ORIENTED_EDGE('',*,*,#3550,.F.);
#5006=ORIENTED_EDGE('',*,*,#3563,.F.);
#5007=ORIENTED_EDGE('',*,*,#3557,.F.);
#5008=ORIENTED_EDGE('',*,*,#3566,.T.);
#5009=ORIENTED_EDGE('',*,*,#3551,.F.);
#5010=ORIENTED_EDGE('',*,*,#3565,.F.);
#5011=ORIENTED_EDGE('',*,*,#3556,.F.);
#5012=ORIENTED_EDGE('',*,*,#3564,.T.);
#5013=ORIENTED_EDGE('',*,*,#3552,.F.);
#5014=ORIENTED_EDGE('',*,*,#3566,.F.);
#5015=ORIENTED_EDGE('',*,*,#3567,.F.);
#5016=ORIENTED_EDGE('',*,*,#3568,.T.);
#5017=ORIENTED_EDGE('',*,*,#3569,.F.);
#5018=ORIENTED_EDGE('',*,*,#3568,.F.);
#5019=ORIENTED_EDGE('',*,*,#3570,.F.);
#5020=ORIENTED_EDGE('',*,*,#3571,.T.);
#5021=ORIENTED_EDGE('',*,*,#3572,.F.);
#5022=ORIENTED_EDGE('',*,*,#3571,.F.);
#5023=ORIENTED_EDGE('',*,*,#3573,.T.);
#5024=ORIENTED_EDGE('',*,*,#3574,.T.);
#5025=ORIENTED_EDGE('',*,*,#3575,.F.);
#5026=ORIENTED_EDGE('',*,*,#3576,.F.);
#5027=ORIENTED_EDGE('',*,*,#3577,.T.);
#5028=ORIENTED_EDGE('',*,*,#3576,.T.);
#5029=ORIENTED_EDGE('',*,*,#3578,.F.);
#5030=ORIENTED_EDGE('',*,*,#3579,.F.);
#5031=ORIENTED_EDGE('',*,*,#3580,.T.);
#5032=ORIENTED_EDGE('',*,*,#3579,.T.);
#5033=ORIENTED_EDGE('',*,*,#3581,.F.);
#5034=ORIENTED_EDGE('',*,*,#3582,.F.);
#5035=ORIENTED_EDGE('',*,*,#3583,.T.);
#5036=ORIENTED_EDGE('',*,*,#3582,.T.);
#5037=ORIENTED_EDGE('',*,*,#3584,.F.);
#5038=ORIENTED_EDGE('',*,*,#3574,.F.);
#5039=ORIENTED_EDGE('',*,*,#3585,.T.);
#5040=ORIENTED_EDGE('',*,*,#3586,.T.);
#5041=ORIENTED_EDGE('',*,*,#3587,.F.);
#5042=ORIENTED_EDGE('',*,*,#3588,.F.);
#5043=ORIENTED_EDGE('',*,*,#3589,.T.);
#5044=ORIENTED_EDGE('',*,*,#3588,.T.);
#5045=ORIENTED_EDGE('',*,*,#3590,.F.);
#5046=ORIENTED_EDGE('',*,*,#3591,.F.);
#5047=ORIENTED_EDGE('',*,*,#3592,.T.);
#5048=ORIENTED_EDGE('',*,*,#3591,.T.);
#5049=ORIENTED_EDGE('',*,*,#3593,.F.);
#5050=ORIENTED_EDGE('',*,*,#3594,.F.);
#5051=ORIENTED_EDGE('',*,*,#3595,.T.);
#5052=ORIENTED_EDGE('',*,*,#3594,.T.);
#5053=ORIENTED_EDGE('',*,*,#3596,.F.);
#5054=ORIENTED_EDGE('',*,*,#3586,.F.);
#5055=ORIENTED_EDGE('',*,*,#3596,.T.);
#5056=ORIENTED_EDGE('',*,*,#3593,.T.);
#5057=ORIENTED_EDGE('',*,*,#3590,.T.);
#5058=ORIENTED_EDGE('',*,*,#3587,.T.);
#5059=ORIENTED_EDGE('',*,*,#3567,.T.);
#5060=ORIENTED_EDGE('',*,*,#3570,.T.);
#5061=ORIENTED_EDGE('',*,*,#3584,.T.);
#5062=ORIENTED_EDGE('',*,*,#3581,.T.);
#5063=ORIENTED_EDGE('',*,*,#3578,.T.);
#5064=ORIENTED_EDGE('',*,*,#3575,.T.);
#5065=ORIENTED_EDGE('',*,*,#3595,.F.);
#5066=ORIENTED_EDGE('',*,*,#3585,.F.);
#5067=ORIENTED_EDGE('',*,*,#3589,.F.);
#5068=ORIENTED_EDGE('',*,*,#3592,.F.);
#5069=ORIENTED_EDGE('',*,*,#3569,.T.);
#5070=ORIENTED_EDGE('',*,*,#3572,.T.);
#5071=ORIENTED_EDGE('',*,*,#3583,.F.);
#5072=ORIENTED_EDGE('',*,*,#3573,.F.);
#5073=ORIENTED_EDGE('',*,*,#3577,.F.);
#5074=ORIENTED_EDGE('',*,*,#3580,.F.);
#5075=ORIENTED_EDGE('',*,*,#3597,.F.);
#5076=ORIENTED_EDGE('',*,*,#3598,.T.);
#5077=ORIENTED_EDGE('',*,*,#3599,.F.);
#5078=ORIENTED_EDGE('',*,*,#3598,.F.);
#5079=ORIENTED_EDGE('',*,*,#3600,.F.);
#5080=ORIENTED_EDGE('',*,*,#3601,.T.);
#5081=ORIENTED_EDGE('',*,*,#3602,.F.);
#5082=ORIENTED_EDGE('',*,*,#3601,.F.);
#5083=ORIENTED_EDGE('',*,*,#3603,.F.);
#5084=ORIENTED_EDGE('',*,*,#3604,.T.);
#5085=ORIENTED_EDGE('',*,*,#3605,.F.);
#5086=ORIENTED_EDGE('',*,*,#3604,.F.);
#5087=ORIENTED_EDGE('',*,*,#3606,.F.);
#5088=ORIENTED_EDGE('',*,*,#3607,.T.);
#5089=ORIENTED_EDGE('',*,*,#3608,.F.);
#5090=ORIENTED_EDGE('',*,*,#3607,.F.);
#5091=ORIENTED_EDGE('',*,*,#3609,.F.);
#5092=ORIENTED_EDGE('',*,*,#3610,.T.);
#5093=ORIENTED_EDGE('',*,*,#3611,.F.);
#5094=ORIENTED_EDGE('',*,*,#3612,.F.);
#5095=ORIENTED_EDGE('',*,*,#3613,.F.);
#5096=ORIENTED_EDGE('',*,*,#3614,.T.);
#5097=ORIENTED_EDGE('',*,*,#3615,.F.);
#5098=ORIENTED_EDGE('',*,*,#3610,.F.);
#5099=ORIENTED_EDGE('',*,*,#3616,.F.);
#5100=ORIENTED_EDGE('',*,*,#3617,.T.);
#5101=ORIENTED_EDGE('',*,*,#3618,.F.);
#5102=ORIENTED_EDGE('',*,*,#3614,.F.);
#5103=ORIENTED_EDGE('',*,*,#3619,.F.);
#5104=ORIENTED_EDGE('',*,*,#3612,.T.);
#5105=ORIENTED_EDGE('',*,*,#3620,.F.);
#5106=ORIENTED_EDGE('',*,*,#3617,.F.);
#5107=ORIENTED_EDGE('',*,*,#3621,.F.);
#5108=ORIENTED_EDGE('',*,*,#3622,.T.);
#5109=ORIENTED_EDGE('',*,*,#3623,.F.);
#5110=ORIENTED_EDGE('',*,*,#3624,.F.);
#5111=ORIENTED_EDGE('',*,*,#3625,.F.);
#5112=ORIENTED_EDGE('',*,*,#3626,.T.);
#5113=ORIENTED_EDGE('',*,*,#3627,.F.);
#5114=ORIENTED_EDGE('',*,*,#3622,.F.);
#5115=ORIENTED_EDGE('',*,*,#3628,.F.);
#5116=ORIENTED_EDGE('',*,*,#3629,.T.);
#5117=ORIENTED_EDGE('',*,*,#3630,.F.);
#5118=ORIENTED_EDGE('',*,*,#3626,.F.);
#5119=ORIENTED_EDGE('',*,*,#3631,.F.);
#5120=ORIENTED_EDGE('',*,*,#3624,.T.);
#5121=ORIENTED_EDGE('',*,*,#3632,.F.);
#5122=ORIENTED_EDGE('',*,*,#3629,.F.);
#5123=ORIENTED_EDGE('',*,*,#3633,.F.);
#5124=ORIENTED_EDGE('',*,*,#3634,.T.);
#5125=ORIENTED_EDGE('',*,*,#3635,.F.);
#5126=ORIENTED_EDGE('',*,*,#3636,.F.);
#5127=ORIENTED_EDGE('',*,*,#3637,.F.);
#5128=ORIENTED_EDGE('',*,*,#3638,.T.);
#5129=ORIENTED_EDGE('',*,*,#3639,.F.);
#5130=ORIENTED_EDGE('',*,*,#3634,.F.);
#5131=ORIENTED_EDGE('',*,*,#3640,.F.);
#5132=ORIENTED_EDGE('',*,*,#3641,.T.);
#5133=ORIENTED_EDGE('',*,*,#3642,.F.);
#5134=ORIENTED_EDGE('',*,*,#3638,.F.);
#5135=ORIENTED_EDGE('',*,*,#3643,.F.);
#5136=ORIENTED_EDGE('',*,*,#3636,.T.);
#5137=ORIENTED_EDGE('',*,*,#3644,.F.);
#5138=ORIENTED_EDGE('',*,*,#3641,.F.);
#5139=ORIENTED_EDGE('',*,*,#3645,.T.);
#5140=ORIENTED_EDGE('',*,*,#3646,.T.);
#5141=ORIENTED_EDGE('',*,*,#3647,.F.);
#5142=ORIENTED_EDGE('',*,*,#3648,.F.);
#5143=ORIENTED_EDGE('',*,*,#3649,.T.);
#5144=ORIENTED_EDGE('',*,*,#3648,.T.);
#5145=ORIENTED_EDGE('',*,*,#3650,.F.);
#5146=ORIENTED_EDGE('',*,*,#3651,.F.);
#5147=ORIENTED_EDGE('',*,*,#3652,.T.);
#5148=ORIENTED_EDGE('',*,*,#3651,.T.);
#5149=ORIENTED_EDGE('',*,*,#3653,.F.);
#5150=ORIENTED_EDGE('',*,*,#3654,.F.);
#5151=ORIENTED_EDGE('',*,*,#3655,.T.);
#5152=ORIENTED_EDGE('',*,*,#3654,.T.);
#5153=ORIENTED_EDGE('',*,*,#3656,.F.);
#5154=ORIENTED_EDGE('',*,*,#3646,.F.);
#5155=ORIENTED_EDGE('',*,*,#3656,.T.);
#5156=ORIENTED_EDGE('',*,*,#3653,.T.);
#5157=ORIENTED_EDGE('',*,*,#3650,.T.);
#5158=ORIENTED_EDGE('',*,*,#3647,.T.);
#5159=ORIENTED_EDGE('',*,*,#3633,.T.);
#5160=ORIENTED_EDGE('',*,*,#3643,.T.);
#5161=ORIENTED_EDGE('',*,*,#3640,.T.);
#5162=ORIENTED_EDGE('',*,*,#3637,.T.);
#5163=ORIENTED_EDGE('',*,*,#3621,.T.);
#5164=ORIENTED_EDGE('',*,*,#3631,.T.);
#5165=ORIENTED_EDGE('',*,*,#3628,.T.);
#5166=ORIENTED_EDGE('',*,*,#3625,.T.);
#5167=ORIENTED_EDGE('',*,*,#3609,.T.);
#5168=ORIENTED_EDGE('',*,*,#3619,.T.);
#5169=ORIENTED_EDGE('',*,*,#3616,.T.);
#5170=ORIENTED_EDGE('',*,*,#3613,.T.);
#5171=ORIENTED_EDGE('',*,*,#3606,.T.);
#5172=ORIENTED_EDGE('',*,*,#3603,.T.);
#5173=ORIENTED_EDGE('',*,*,#3600,.T.);
#5174=ORIENTED_EDGE('',*,*,#3597,.T.);
#5175=ORIENTED_EDGE('',*,*,#3655,.F.);
#5176=ORIENTED_EDGE('',*,*,#3645,.F.);
#5177=ORIENTED_EDGE('',*,*,#3649,.F.);
#5178=ORIENTED_EDGE('',*,*,#3652,.F.);
#5179=ORIENTED_EDGE('',*,*,#3635,.T.);
#5180=ORIENTED_EDGE('',*,*,#3639,.T.);
#5181=ORIENTED_EDGE('',*,*,#3642,.T.);
#5182=ORIENTED_EDGE('',*,*,#3644,.T.);
#5183=ORIENTED_EDGE('',*,*,#3623,.T.);
#5184=ORIENTED_EDGE('',*,*,#3627,.T.);
#5185=ORIENTED_EDGE('',*,*,#3630,.T.);
#5186=ORIENTED_EDGE('',*,*,#3632,.T.);
#5187=ORIENTED_EDGE('',*,*,#3611,.T.);
#5188=ORIENTED_EDGE('',*,*,#3615,.T.);
#5189=ORIENTED_EDGE('',*,*,#3618,.T.);
#5190=ORIENTED_EDGE('',*,*,#3620,.T.);
#5191=ORIENTED_EDGE('',*,*,#3608,.T.);
#5192=ORIENTED_EDGE('',*,*,#3605,.T.);
#5193=ORIENTED_EDGE('',*,*,#3602,.T.);
#5194=ORIENTED_EDGE('',*,*,#3599,.T.);
#5195=ORIENTED_EDGE('',*,*,#3657,.F.);
#5196=ORIENTED_EDGE('',*,*,#3658,.T.);
#5197=ORIENTED_EDGE('',*,*,#3659,.F.);
#5198=ORIENTED_EDGE('',*,*,#3658,.F.);
#5199=ORIENTED_EDGE('',*,*,#3660,.T.);
#5200=ORIENTED_EDGE('',*,*,#3661,.T.);
#5201=ORIENTED_EDGE('',*,*,#3662,.F.);
#5202=ORIENTED_EDGE('',*,*,#3663,.F.);
#5203=ORIENTED_EDGE('',*,*,#3657,.T.);
#5204=ORIENTED_EDGE('',*,*,#3664,.T.);
#5205=ORIENTED_EDGE('',*,*,#3663,.T.);
#5206=ORIENTED_EDGE('',*,*,#3665,.F.);
#5207=ORIENTED_EDGE('',*,*,#3666,.F.);
#5208=ORIENTED_EDGE('',*,*,#3667,.T.);
#5209=ORIENTED_EDGE('',*,*,#3666,.T.);
#5210=ORIENTED_EDGE('',*,*,#3668,.F.);
#5211=ORIENTED_EDGE('',*,*,#3669,.F.);
#5212=ORIENTED_EDGE('',*,*,#3659,.T.);
#5213=ORIENTED_EDGE('',*,*,#3670,.T.);
#5214=ORIENTED_EDGE('',*,*,#3669,.T.);
#5215=ORIENTED_EDGE('',*,*,#3671,.F.);
#5216=ORIENTED_EDGE('',*,*,#3661,.F.);
#5217=ORIENTED_EDGE('',*,*,#3671,.T.);
#5218=ORIENTED_EDGE('',*,*,#3668,.T.);
#5219=ORIENTED_EDGE('',*,*,#3665,.T.);
#5220=ORIENTED_EDGE('',*,*,#3662,.T.);
#5221=ORIENTED_EDGE('',*,*,#3670,.F.);
#5222=ORIENTED_EDGE('',*,*,#3660,.F.);
#5223=ORIENTED_EDGE('',*,*,#3664,.F.);
#5224=ORIENTED_EDGE('',*,*,#3667,.F.);
#5225=ORIENTED_EDGE('',*,*,#3672,.F.);
#5226=ORIENTED_EDGE('',*,*,#3673,.T.);
#5227=ORIENTED_EDGE('',*,*,#3674,.F.);
#5228=ORIENTED_EDGE('',*,*,#3673,.F.);
#5229=ORIENTED_EDGE('',*,*,#3675,.T.);
#5230=ORIENTED_EDGE('',*,*,#3676,.T.);
#5231=ORIENTED_EDGE('',*,*,#3677,.F.);
#5232=ORIENTED_EDGE('',*,*,#3678,.F.);
#5233=ORIENTED_EDGE('',*,*,#3672,.T.);
#5234=ORIENTED_EDGE('',*,*,#3679,.T.);
#5235=ORIENTED_EDGE('',*,*,#3678,.T.);
#5236=ORIENTED_EDGE('',*,*,#3680,.F.);
#5237=ORIENTED_EDGE('',*,*,#3681,.F.);
#5238=ORIENTED_EDGE('',*,*,#3682,.T.);
#5239=ORIENTED_EDGE('',*,*,#3681,.T.);
#5240=ORIENTED_EDGE('',*,*,#3683,.F.);
#5241=ORIENTED_EDGE('',*,*,#3684,.F.);
#5242=ORIENTED_EDGE('',*,*,#3674,.T.);
#5243=ORIENTED_EDGE('',*,*,#3685,.T.);
#5244=ORIENTED_EDGE('',*,*,#3684,.T.);
#5245=ORIENTED_EDGE('',*,*,#3686,.F.);
#5246=ORIENTED_EDGE('',*,*,#3676,.F.);
#5247=ORIENTED_EDGE('',*,*,#3686,.T.);
#5248=ORIENTED_EDGE('',*,*,#3683,.T.);
#5249=ORIENTED_EDGE('',*,*,#3680,.T.);
#5250=ORIENTED_EDGE('',*,*,#3677,.T.);
#5251=ORIENTED_EDGE('',*,*,#3685,.F.);
#5252=ORIENTED_EDGE('',*,*,#3675,.F.);
#5253=ORIENTED_EDGE('',*,*,#3679,.F.);
#5254=ORIENTED_EDGE('',*,*,#3682,.F.);
#5255=ORIENTED_EDGE('',*,*,#3687,.F.);
#5256=ORIENTED_EDGE('',*,*,#3688,.T.);
#5257=ORIENTED_EDGE('',*,*,#3689,.T.);
#5258=ORIENTED_EDGE('',*,*,#3690,.T.);
#5259=ORIENTED_EDGE('',*,*,#3691,.F.);
#5260=ORIENTED_EDGE('',*,*,#3692,.T.);
#5261=ORIENTED_EDGE('',*,*,#3687,.T.);
#5262=ORIENTED_EDGE('',*,*,#3693,.T.);
#5263=ORIENTED_EDGE('',*,*,#3694,.F.);
#5264=ORIENTED_EDGE('',*,*,#3695,.T.);
#5265=ORIENTED_EDGE('',*,*,#3691,.T.);
#5266=ORIENTED_EDGE('',*,*,#3696,.T.);
#5267=ORIENTED_EDGE('',*,*,#3697,.F.);
#5268=ORIENTED_EDGE('',*,*,#3698,.T.);
#5269=ORIENTED_EDGE('',*,*,#3694,.T.);
#5270=ORIENTED_EDGE('',*,*,#3699,.T.);
#5271=ORIENTED_EDGE('',*,*,#3700,.F.);
#5272=ORIENTED_EDGE('',*,*,#3701,.T.);
#5273=ORIENTED_EDGE('',*,*,#3697,.T.);
#5274=ORIENTED_EDGE('',*,*,#3702,.T.);
#5275=ORIENTED_EDGE('',*,*,#3703,.F.);
#5276=ORIENTED_EDGE('',*,*,#3704,.T.);
#5277=ORIENTED_EDGE('',*,*,#3700,.T.);
#5278=ORIENTED_EDGE('',*,*,#3705,.T.);
#5279=ORIENTED_EDGE('',*,*,#3706,.F.);
#5280=ORIENTED_EDGE('',*,*,#3707,.T.);
#5281=ORIENTED_EDGE('',*,*,#3703,.T.);
#5282=ORIENTED_EDGE('',*,*,#3708,.T.);
#5283=ORIENTED_EDGE('',*,*,#3709,.F.);
#5284=ORIENTED_EDGE('',*,*,#3710,.T.);
#5285=ORIENTED_EDGE('',*,*,#3706,.T.);
#5286=ORIENTED_EDGE('',*,*,#3711,.T.);
#5287=ORIENTED_EDGE('',*,*,#3712,.F.);
#5288=ORIENTED_EDGE('',*,*,#3713,.T.);
#5289=ORIENTED_EDGE('',*,*,#3709,.T.);
#5290=ORIENTED_EDGE('',*,*,#3714,.T.);
#5291=ORIENTED_EDGE('',*,*,#3715,.F.);
#5292=ORIENTED_EDGE('',*,*,#3716,.T.);
#5293=ORIENTED_EDGE('',*,*,#3712,.T.);
#5294=ORIENTED_EDGE('',*,*,#3717,.T.);
#5295=ORIENTED_EDGE('',*,*,#3718,.F.);
#5296=ORIENTED_EDGE('',*,*,#3719,.T.);
#5297=ORIENTED_EDGE('',*,*,#3720,.T.);
#5298=ORIENTED_EDGE('',*,*,#3721,.F.);
#5299=ORIENTED_EDGE('',*,*,#3722,.F.);
#5300=ORIENTED_EDGE('',*,*,#3723,.T.);
#5301=ORIENTED_EDGE('',*,*,#3718,.T.);
#5302=ORIENTED_EDGE('',*,*,#3724,.F.);
#5303=ORIENTED_EDGE('',*,*,#3725,.F.);
#5304=ORIENTED_EDGE('',*,*,#3726,.T.);
#5305=ORIENTED_EDGE('',*,*,#3722,.T.);
#5306=ORIENTED_EDGE('',*,*,#3727,.F.);
#5307=ORIENTED_EDGE('',*,*,#3728,.F.);
#5308=ORIENTED_EDGE('',*,*,#3729,.T.);
#5309=ORIENTED_EDGE('',*,*,#3725,.T.);
#5310=ORIENTED_EDGE('',*,*,#3730,.F.);
#5311=ORIENTED_EDGE('',*,*,#3731,.F.);
#5312=ORIENTED_EDGE('',*,*,#3732,.T.);
#5313=ORIENTED_EDGE('',*,*,#3728,.T.);
#5314=ORIENTED_EDGE('',*,*,#3733,.F.);
#5315=ORIENTED_EDGE('',*,*,#3734,.F.);
#5316=ORIENTED_EDGE('',*,*,#3735,.T.);
#5317=ORIENTED_EDGE('',*,*,#3731,.T.);
#5318=ORIENTED_EDGE('',*,*,#3736,.F.);
#5319=ORIENTED_EDGE('',*,*,#3737,.F.);
#5320=ORIENTED_EDGE('',*,*,#3738,.T.);
#5321=ORIENTED_EDGE('',*,*,#3734,.T.);
#5322=ORIENTED_EDGE('',*,*,#3739,.F.);
#5323=ORIENTED_EDGE('',*,*,#3740,.F.);
#5324=ORIENTED_EDGE('',*,*,#3741,.T.);
#5325=ORIENTED_EDGE('',*,*,#3737,.T.);
#5326=ORIENTED_EDGE('',*,*,#3742,.F.);
#5327=ORIENTED_EDGE('',*,*,#3743,.F.);
#5328=ORIENTED_EDGE('',*,*,#3744,.T.);
#5329=ORIENTED_EDGE('',*,*,#3740,.T.);
#5330=ORIENTED_EDGE('',*,*,#3745,.F.);
#5331=ORIENTED_EDGE('',*,*,#3746,.F.);
#5332=ORIENTED_EDGE('',*,*,#3747,.T.);
#5333=ORIENTED_EDGE('',*,*,#3743,.T.);
#5334=ORIENTED_EDGE('',*,*,#3748,.F.);
#5335=ORIENTED_EDGE('',*,*,#3749,.F.);
#5336=ORIENTED_EDGE('',*,*,#3720,.F.);
#5337=ORIENTED_EDGE('',*,*,#3750,.F.);
#5338=ORIENTED_EDGE('',*,*,#3751,.F.);
#5339=ORIENTED_EDGE('',*,*,#3752,.F.);
#5340=ORIENTED_EDGE('',*,*,#3753,.T.);
#5341=ORIENTED_EDGE('',*,*,#3754,.F.);
#5342=ORIENTED_EDGE('',*,*,#3753,.F.);
#5343=ORIENTED_EDGE('',*,*,#3750,.T.);
#5344=ORIENTED_EDGE('',*,*,#3719,.F.);
#5345=ORIENTED_EDGE('',*,*,#3723,.F.);
#5346=ORIENTED_EDGE('',*,*,#3726,.F.);
#5347=ORIENTED_EDGE('',*,*,#3729,.F.);
#5348=ORIENTED_EDGE('',*,*,#3732,.F.);
#5349=ORIENTED_EDGE('',*,*,#3735,.F.);
#5350=ORIENTED_EDGE('',*,*,#3738,.F.);
#5351=ORIENTED_EDGE('',*,*,#3741,.F.);
#5352=ORIENTED_EDGE('',*,*,#3744,.F.);
#5353=ORIENTED_EDGE('',*,*,#3747,.F.);
#5354=ORIENTED_EDGE('',*,*,#3755,.F.);
#5355=ORIENTED_EDGE('',*,*,#3756,.F.);
#5356=ORIENTED_EDGE('',*,*,#3688,.F.);
#5357=ORIENTED_EDGE('',*,*,#3692,.F.);
#5358=ORIENTED_EDGE('',*,*,#3695,.F.);
#5359=ORIENTED_EDGE('',*,*,#3698,.F.);
#5360=ORIENTED_EDGE('',*,*,#3701,.F.);
#5361=ORIENTED_EDGE('',*,*,#3704,.F.);
#5362=ORIENTED_EDGE('',*,*,#3707,.F.);
#5363=ORIENTED_EDGE('',*,*,#3710,.F.);
#5364=ORIENTED_EDGE('',*,*,#3713,.F.);
#5365=ORIENTED_EDGE('',*,*,#3716,.F.);
#5366=ORIENTED_EDGE('',*,*,#3757,.F.);
#5367=ORIENTED_EDGE('',*,*,#3746,.T.);
#5368=ORIENTED_EDGE('',*,*,#3758,.F.);
#5369=ORIENTED_EDGE('',*,*,#3759,.F.);
#5370=ORIENTED_EDGE('',*,*,#3755,.T.);
#5371=ORIENTED_EDGE('',*,*,#3749,.T.);
#5372=ORIENTED_EDGE('',*,*,#3752,.T.);
#5373=ORIENTED_EDGE('',*,*,#3760,.F.);
#5374=ORIENTED_EDGE('',*,*,#3717,.F.);
#5375=ORIENTED_EDGE('',*,*,#3714,.F.);
#5376=ORIENTED_EDGE('',*,*,#3711,.F.);
#5377=ORIENTED_EDGE('',*,*,#3708,.F.);
#5378=ORIENTED_EDGE('',*,*,#3705,.F.);
#5379=ORIENTED_EDGE('',*,*,#3702,.F.);
#5380=ORIENTED_EDGE('',*,*,#3699,.F.);
#5381=ORIENTED_EDGE('',*,*,#3696,.F.);
#5382=ORIENTED_EDGE('',*,*,#3693,.F.);
#5383=ORIENTED_EDGE('',*,*,#3690,.F.);
#5384=ORIENTED_EDGE('',*,*,#3761,.F.);
#5385=ORIENTED_EDGE('',*,*,#3758,.T.);
#5386=ORIENTED_EDGE('',*,*,#3748,.T.);
#5387=ORIENTED_EDGE('',*,*,#3745,.T.);
#5388=ORIENTED_EDGE('',*,*,#3742,.T.);
#5389=ORIENTED_EDGE('',*,*,#3739,.T.);
#5390=ORIENTED_EDGE('',*,*,#3736,.T.);
#5391=ORIENTED_EDGE('',*,*,#3733,.T.);
#5392=ORIENTED_EDGE('',*,*,#3730,.T.);
#5393=ORIENTED_EDGE('',*,*,#3727,.T.);
#5394=ORIENTED_EDGE('',*,*,#3724,.T.);
#5395=ORIENTED_EDGE('',*,*,#3721,.T.);
#5396=ORIENTED_EDGE('',*,*,#3715,.T.);
#5397=ORIENTED_EDGE('',*,*,#3760,.T.);
#5398=ORIENTED_EDGE('',*,*,#3751,.T.);
#5399=ORIENTED_EDGE('',*,*,#3757,.T.);
#5400=ORIENTED_EDGE('',*,*,#3762,.F.);
#5401=ORIENTED_EDGE('',*,*,#3763,.T.);
#5402=ORIENTED_EDGE('',*,*,#3764,.T.);
#5403=ORIENTED_EDGE('',*,*,#3765,.F.);
#5404=ORIENTED_EDGE('',*,*,#3766,.F.);
#5405=ORIENTED_EDGE('',*,*,#3767,.T.);
#5406=ORIENTED_EDGE('',*,*,#3768,.T.);
#5407=ORIENTED_EDGE('',*,*,#3763,.F.);
#5408=ORIENTED_EDGE('',*,*,#3769,.F.);
#5409=ORIENTED_EDGE('',*,*,#3770,.T.);
#5410=ORIENTED_EDGE('',*,*,#3771,.T.);
#5411=ORIENTED_EDGE('',*,*,#3767,.F.);
#5412=ORIENTED_EDGE('',*,*,#3772,.F.);
#5413=ORIENTED_EDGE('',*,*,#3773,.T.);
#5414=ORIENTED_EDGE('',*,*,#3774,.T.);
#5415=ORIENTED_EDGE('',*,*,#3770,.F.);
#5416=ORIENTED_EDGE('',*,*,#3775,.F.);
#5417=ORIENTED_EDGE('',*,*,#3776,.T.);
#5418=ORIENTED_EDGE('',*,*,#3777,.T.);
#5419=ORIENTED_EDGE('',*,*,#3773,.F.);
#5420=ORIENTED_EDGE('',*,*,#3778,.F.);
#5421=ORIENTED_EDGE('',*,*,#3765,.T.);
#5422=ORIENTED_EDGE('',*,*,#3779,.T.);
#5423=ORIENTED_EDGE('',*,*,#3776,.F.);
#5424=ORIENTED_EDGE('',*,*,#3779,.F.);
#5425=ORIENTED_EDGE('',*,*,#3764,.F.);
#5426=ORIENTED_EDGE('',*,*,#3768,.F.);
#5427=ORIENTED_EDGE('',*,*,#3771,.F.);
#5428=ORIENTED_EDGE('',*,*,#3774,.F.);
#5429=ORIENTED_EDGE('',*,*,#3777,.F.);
#5430=ORIENTED_EDGE('',*,*,#3780,.T.);
#5431=ORIENTED_EDGE('',*,*,#3756,.T.);
#5432=ORIENTED_EDGE('',*,*,#3759,.T.);
#5433=ORIENTED_EDGE('',*,*,#3761,.T.);
#5434=ORIENTED_EDGE('',*,*,#3689,.F.);
#5435=ORIENTED_EDGE('',*,*,#3780,.F.);
#5436=ORIENTED_EDGE('',*,*,#3781,.T.);
#5437=ORIENTED_EDGE('',*,*,#3782,.T.);
#5438=ORIENTED_EDGE('',*,*,#3781,.F.);
#5439=ORIENTED_EDGE('',*,*,#3782,.F.);
#5440=ORIENTED_EDGE('',*,*,#3762,.T.);
#5441=ORIENTED_EDGE('',*,*,#3778,.T.);
#5442=ORIENTED_EDGE('',*,*,#3775,.T.);
#5443=ORIENTED_EDGE('',*,*,#3772,.T.);
#5444=ORIENTED_EDGE('',*,*,#3769,.T.);
#5445=ORIENTED_EDGE('',*,*,#3766,.T.);
#5446=ORIENTED_EDGE('',*,*,#3754,.T.);
#5447=ORIENTED_EDGE('',*,*,#3783,.F.);
#5448=ORIENTED_EDGE('',*,*,#3784,.T.);
#5449=ORIENTED_EDGE('',*,*,#3785,.T.);
#5450=ORIENTED_EDGE('',*,*,#3786,.T.);
#5451=ORIENTED_EDGE('',*,*,#3787,.F.);
#5452=ORIENTED_EDGE('',*,*,#3788,.T.);
#5453=ORIENTED_EDGE('',*,*,#3783,.T.);
#5454=ORIENTED_EDGE('',*,*,#3789,.T.);
#5455=ORIENTED_EDGE('',*,*,#3790,.F.);
#5456=ORIENTED_EDGE('',*,*,#3791,.T.);
#5457=ORIENTED_EDGE('',*,*,#3787,.T.);
#5458=ORIENTED_EDGE('',*,*,#3792,.T.);
#5459=ORIENTED_EDGE('',*,*,#3793,.F.);
#5460=ORIENTED_EDGE('',*,*,#3794,.T.);
#5461=ORIENTED_EDGE('',*,*,#3790,.T.);
#5462=ORIENTED_EDGE('',*,*,#3795,.T.);
#5463=ORIENTED_EDGE('',*,*,#3796,.F.);
#5464=ORIENTED_EDGE('',*,*,#3797,.T.);
#5465=ORIENTED_EDGE('',*,*,#3793,.T.);
#5466=ORIENTED_EDGE('',*,*,#3798,.T.);
#5467=ORIENTED_EDGE('',*,*,#3799,.F.);
#5468=ORIENTED_EDGE('',*,*,#3800,.T.);
#5469=ORIENTED_EDGE('',*,*,#3796,.T.);
#5470=ORIENTED_EDGE('',*,*,#3801,.T.);
#5471=ORIENTED_EDGE('',*,*,#3802,.F.);
#5472=ORIENTED_EDGE('',*,*,#3803,.T.);
#5473=ORIENTED_EDGE('',*,*,#3799,.T.);
#5474=ORIENTED_EDGE('',*,*,#3804,.T.);
#5475=ORIENTED_EDGE('',*,*,#3805,.F.);
#5476=ORIENTED_EDGE('',*,*,#3806,.T.);
#5477=ORIENTED_EDGE('',*,*,#3802,.T.);
#5478=ORIENTED_EDGE('',*,*,#3807,.T.);
#5479=ORIENTED_EDGE('',*,*,#3808,.F.);
#5480=ORIENTED_EDGE('',*,*,#3809,.T.);
#5481=ORIENTED_EDGE('',*,*,#3805,.T.);
#5482=ORIENTED_EDGE('',*,*,#3810,.T.);
#5483=ORIENTED_EDGE('',*,*,#3811,.F.);
#5484=ORIENTED_EDGE('',*,*,#3812,.T.);
#5485=ORIENTED_EDGE('',*,*,#3808,.T.);
#5486=ORIENTED_EDGE('',*,*,#3813,.T.);
#5487=ORIENTED_EDGE('',*,*,#3814,.F.);
#5488=ORIENTED_EDGE('',*,*,#3815,.T.);
#5489=ORIENTED_EDGE('',*,*,#3811,.T.);
#5490=ORIENTED_EDGE('',*,*,#3816,.T.);
#5491=ORIENTED_EDGE('',*,*,#3817,.F.);
#5492=ORIENTED_EDGE('',*,*,#3818,.T.);
#5493=ORIENTED_EDGE('',*,*,#3814,.T.);
#5494=ORIENTED_EDGE('',*,*,#3819,.T.);
#5495=ORIENTED_EDGE('',*,*,#3820,.F.);
#5496=ORIENTED_EDGE('',*,*,#3821,.T.);
#5497=ORIENTED_EDGE('',*,*,#3817,.T.);
#5498=ORIENTED_EDGE('',*,*,#3822,.T.);
#5499=ORIENTED_EDGE('',*,*,#3823,.F.);
#5500=ORIENTED_EDGE('',*,*,#3824,.T.);
#5501=ORIENTED_EDGE('',*,*,#3820,.T.);
#5502=ORIENTED_EDGE('',*,*,#3825,.T.);
#5503=ORIENTED_EDGE('',*,*,#3826,.F.);
#5504=ORIENTED_EDGE('',*,*,#3827,.T.);
#5505=ORIENTED_EDGE('',*,*,#3823,.T.);
#5506=ORIENTED_EDGE('',*,*,#3828,.T.);
#5507=ORIENTED_EDGE('',*,*,#3829,.F.);
#5508=ORIENTED_EDGE('',*,*,#3830,.T.);
#5509=ORIENTED_EDGE('',*,*,#3831,.T.);
#5510=ORIENTED_EDGE('',*,*,#3832,.F.);
#5511=ORIENTED_EDGE('',*,*,#3833,.F.);
#5512=ORIENTED_EDGE('',*,*,#3834,.T.);
#5513=ORIENTED_EDGE('',*,*,#3829,.T.);
#5514=ORIENTED_EDGE('',*,*,#3835,.F.);
#5515=ORIENTED_EDGE('',*,*,#3836,.F.);
#5516=ORIENTED_EDGE('',*,*,#3837,.T.);
#5517=ORIENTED_EDGE('',*,*,#3833,.T.);
#5518=ORIENTED_EDGE('',*,*,#3838,.F.);
#5519=ORIENTED_EDGE('',*,*,#3839,.F.);
#5520=ORIENTED_EDGE('',*,*,#3840,.T.);
#5521=ORIENTED_EDGE('',*,*,#3836,.T.);
#5522=ORIENTED_EDGE('',*,*,#3841,.F.);
#5523=ORIENTED_EDGE('',*,*,#3842,.F.);
#5524=ORIENTED_EDGE('',*,*,#3843,.T.);
#5525=ORIENTED_EDGE('',*,*,#3839,.T.);
#5526=ORIENTED_EDGE('',*,*,#3844,.F.);
#5527=ORIENTED_EDGE('',*,*,#3845,.F.);
#5528=ORIENTED_EDGE('',*,*,#3846,.T.);
#5529=ORIENTED_EDGE('',*,*,#3842,.T.);
#5530=ORIENTED_EDGE('',*,*,#3847,.F.);
#5531=ORIENTED_EDGE('',*,*,#3848,.F.);
#5532=ORIENTED_EDGE('',*,*,#3849,.T.);
#5533=ORIENTED_EDGE('',*,*,#3845,.T.);
#5534=ORIENTED_EDGE('',*,*,#3850,.F.);
#5535=ORIENTED_EDGE('',*,*,#3851,.F.);
#5536=ORIENTED_EDGE('',*,*,#3852,.T.);
#5537=ORIENTED_EDGE('',*,*,#3848,.T.);
#5538=ORIENTED_EDGE('',*,*,#3853,.F.);
#5539=ORIENTED_EDGE('',*,*,#3854,.F.);
#5540=ORIENTED_EDGE('',*,*,#3855,.T.);
#5541=ORIENTED_EDGE('',*,*,#3851,.T.);
#5542=ORIENTED_EDGE('',*,*,#3856,.F.);
#5543=ORIENTED_EDGE('',*,*,#3857,.F.);
#5544=ORIENTED_EDGE('',*,*,#3858,.T.);
#5545=ORIENTED_EDGE('',*,*,#3854,.T.);
#5546=ORIENTED_EDGE('',*,*,#3859,.F.);
#5547=ORIENTED_EDGE('',*,*,#3860,.F.);
#5548=ORIENTED_EDGE('',*,*,#3861,.T.);
#5549=ORIENTED_EDGE('',*,*,#3857,.T.);
#5550=ORIENTED_EDGE('',*,*,#3862,.F.);
#5551=ORIENTED_EDGE('',*,*,#3863,.F.);
#5552=ORIENTED_EDGE('',*,*,#3864,.T.);
#5553=ORIENTED_EDGE('',*,*,#3860,.T.);
#5554=ORIENTED_EDGE('',*,*,#3865,.F.);
#5555=ORIENTED_EDGE('',*,*,#3866,.F.);
#5556=ORIENTED_EDGE('',*,*,#3867,.T.);
#5557=ORIENTED_EDGE('',*,*,#3863,.T.);
#5558=ORIENTED_EDGE('',*,*,#3868,.F.);
#5559=ORIENTED_EDGE('',*,*,#3869,.F.);
#5560=ORIENTED_EDGE('',*,*,#3870,.T.);
#5561=ORIENTED_EDGE('',*,*,#3866,.T.);
#5562=ORIENTED_EDGE('',*,*,#3871,.F.);
#5563=ORIENTED_EDGE('',*,*,#3872,.F.);
#5564=ORIENTED_EDGE('',*,*,#3873,.T.);
#5565=ORIENTED_EDGE('',*,*,#3869,.T.);
#5566=ORIENTED_EDGE('',*,*,#3874,.F.);
#5567=ORIENTED_EDGE('',*,*,#3875,.F.);
#5568=ORIENTED_EDGE('',*,*,#3831,.F.);
#5569=ORIENTED_EDGE('',*,*,#3876,.F.);
#5570=ORIENTED_EDGE('',*,*,#3877,.F.);
#5571=ORIENTED_EDGE('',*,*,#3878,.F.);
#5572=ORIENTED_EDGE('',*,*,#3879,.T.);
#5573=ORIENTED_EDGE('',*,*,#3880,.F.);
#5574=ORIENTED_EDGE('',*,*,#3879,.F.);
#5575=ORIENTED_EDGE('',*,*,#3876,.T.);
#5576=ORIENTED_EDGE('',*,*,#3830,.F.);
#5577=ORIENTED_EDGE('',*,*,#3834,.F.);
#5578=ORIENTED_EDGE('',*,*,#3837,.F.);
#5579=ORIENTED_EDGE('',*,*,#3840,.F.);
#5580=ORIENTED_EDGE('',*,*,#3843,.F.);
#5581=ORIENTED_EDGE('',*,*,#3846,.F.);
#5582=ORIENTED_EDGE('',*,*,#3849,.F.);
#5583=ORIENTED_EDGE('',*,*,#3852,.F.);
#5584=ORIENTED_EDGE('',*,*,#3855,.F.);
#5585=ORIENTED_EDGE('',*,*,#3858,.F.);
#5586=ORIENTED_EDGE('',*,*,#3861,.F.);
#5587=ORIENTED_EDGE('',*,*,#3864,.F.);
#5588=ORIENTED_EDGE('',*,*,#3867,.F.);
#5589=ORIENTED_EDGE('',*,*,#3870,.F.);
#5590=ORIENTED_EDGE('',*,*,#3873,.F.);
#5591=ORIENTED_EDGE('',*,*,#3881,.F.);
#5592=ORIENTED_EDGE('',*,*,#3882,.F.);
#5593=ORIENTED_EDGE('',*,*,#3784,.F.);
#5594=ORIENTED_EDGE('',*,*,#3788,.F.);
#5595=ORIENTED_EDGE('',*,*,#3791,.F.);
#5596=ORIENTED_EDGE('',*,*,#3794,.F.);
#5597=ORIENTED_EDGE('',*,*,#3797,.F.);
#5598=ORIENTED_EDGE('',*,*,#3800,.F.);
#5599=ORIENTED_EDGE('',*,*,#3803,.F.);
#5600=ORIENTED_EDGE('',*,*,#3806,.F.);
#5601=ORIENTED_EDGE('',*,*,#3809,.F.);
#5602=ORIENTED_EDGE('',*,*,#3812,.F.);
#5603=ORIENTED_EDGE('',*,*,#3815,.F.);
#5604=ORIENTED_EDGE('',*,*,#3818,.F.);
#5605=ORIENTED_EDGE('',*,*,#3821,.F.);
#5606=ORIENTED_EDGE('',*,*,#3824,.F.);
#5607=ORIENTED_EDGE('',*,*,#3827,.F.);
#5608=ORIENTED_EDGE('',*,*,#3883,.F.);
#5609=ORIENTED_EDGE('',*,*,#3872,.T.);
#5610=ORIENTED_EDGE('',*,*,#3884,.F.);
#5611=ORIENTED_EDGE('',*,*,#3885,.F.);
#5612=ORIENTED_EDGE('',*,*,#3881,.T.);
#5613=ORIENTED_EDGE('',*,*,#3875,.T.);
#5614=ORIENTED_EDGE('',*,*,#3878,.T.);
#5615=ORIENTED_EDGE('',*,*,#3886,.F.);
#5616=ORIENTED_EDGE('',*,*,#3828,.F.);
#5617=ORIENTED_EDGE('',*,*,#3825,.F.);
#5618=ORIENTED_EDGE('',*,*,#3822,.F.);
#5619=ORIENTED_EDGE('',*,*,#3819,.F.);
#5620=ORIENTED_EDGE('',*,*,#3816,.F.);
#5621=ORIENTED_EDGE('',*,*,#3813,.F.);
#5622=ORIENTED_EDGE('',*,*,#3810,.F.);
#5623=ORIENTED_EDGE('',*,*,#3807,.F.);
#5624=ORIENTED_EDGE('',*,*,#3804,.F.);
#5625=ORIENTED_EDGE('',*,*,#3801,.F.);
#5626=ORIENTED_EDGE('',*,*,#3798,.F.);
#5627=ORIENTED_EDGE('',*,*,#3795,.F.);
#5628=ORIENTED_EDGE('',*,*,#3792,.F.);
#5629=ORIENTED_EDGE('',*,*,#3789,.F.);
#5630=ORIENTED_EDGE('',*,*,#3786,.F.);
#5631=ORIENTED_EDGE('',*,*,#3887,.F.);
#5632=ORIENTED_EDGE('',*,*,#3884,.T.);
#5633=ORIENTED_EDGE('',*,*,#3874,.T.);
#5634=ORIENTED_EDGE('',*,*,#3871,.T.);
#5635=ORIENTED_EDGE('',*,*,#3868,.T.);
#5636=ORIENTED_EDGE('',*,*,#3865,.T.);
#5637=ORIENTED_EDGE('',*,*,#3862,.T.);
#5638=ORIENTED_EDGE('',*,*,#3859,.T.);
#5639=ORIENTED_EDGE('',*,*,#3856,.T.);
#5640=ORIENTED_EDGE('',*,*,#3853,.T.);
#5641=ORIENTED_EDGE('',*,*,#3850,.T.);
#5642=ORIENTED_EDGE('',*,*,#3847,.T.);
#5643=ORIENTED_EDGE('',*,*,#3844,.T.);
#5644=ORIENTED_EDGE('',*,*,#3841,.T.);
#5645=ORIENTED_EDGE('',*,*,#3838,.T.);
#5646=ORIENTED_EDGE('',*,*,#3835,.T.);
#5647=ORIENTED_EDGE('',*,*,#3832,.T.);
#5648=ORIENTED_EDGE('',*,*,#3826,.T.);
#5649=ORIENTED_EDGE('',*,*,#3886,.T.);
#5650=ORIENTED_EDGE('',*,*,#3877,.T.);
#5651=ORIENTED_EDGE('',*,*,#3883,.T.);
#5652=ORIENTED_EDGE('',*,*,#3888,.F.);
#5653=ORIENTED_EDGE('',*,*,#3889,.T.);
#5654=ORIENTED_EDGE('',*,*,#3890,.T.);
#5655=ORIENTED_EDGE('',*,*,#3891,.F.);
#5656=ORIENTED_EDGE('',*,*,#3892,.F.);
#5657=ORIENTED_EDGE('',*,*,#3893,.T.);
#5658=ORIENTED_EDGE('',*,*,#3894,.T.);
#5659=ORIENTED_EDGE('',*,*,#3889,.F.);
#5660=ORIENTED_EDGE('',*,*,#3895,.F.);
#5661=ORIENTED_EDGE('',*,*,#3896,.T.);
#5662=ORIENTED_EDGE('',*,*,#3897,.T.);
#5663=ORIENTED_EDGE('',*,*,#3893,.F.);
#5664=ORIENTED_EDGE('',*,*,#3898,.F.);
#5665=ORIENTED_EDGE('',*,*,#3899,.T.);
#5666=ORIENTED_EDGE('',*,*,#3900,.T.);
#5667=ORIENTED_EDGE('',*,*,#3896,.F.);
#5668=ORIENTED_EDGE('',*,*,#3901,.F.);
#5669=ORIENTED_EDGE('',*,*,#3902,.T.);
#5670=ORIENTED_EDGE('',*,*,#3903,.T.);
#5671=ORIENTED_EDGE('',*,*,#3899,.F.);
#5672=ORIENTED_EDGE('',*,*,#3904,.F.);
#5673=ORIENTED_EDGE('',*,*,#3891,.T.);
#5674=ORIENTED_EDGE('',*,*,#3905,.T.);
#5675=ORIENTED_EDGE('',*,*,#3902,.F.);
#5676=ORIENTED_EDGE('',*,*,#3905,.F.);
#5677=ORIENTED_EDGE('',*,*,#3890,.F.);
#5678=ORIENTED_EDGE('',*,*,#3894,.F.);
#5679=ORIENTED_EDGE('',*,*,#3897,.F.);
#5680=ORIENTED_EDGE('',*,*,#3900,.F.);
#5681=ORIENTED_EDGE('',*,*,#3903,.F.);
#5682=ORIENTED_EDGE('',*,*,#3906,.T.);
#5683=ORIENTED_EDGE('',*,*,#3882,.T.);
#5684=ORIENTED_EDGE('',*,*,#3885,.T.);
#5685=ORIENTED_EDGE('',*,*,#3887,.T.);
#5686=ORIENTED_EDGE('',*,*,#3785,.F.);
#5687=ORIENTED_EDGE('',*,*,#3906,.F.);
#5688=ORIENTED_EDGE('',*,*,#3907,.T.);
#5689=ORIENTED_EDGE('',*,*,#3908,.T.);
#5690=ORIENTED_EDGE('',*,*,#3907,.F.);
#5691=ORIENTED_EDGE('',*,*,#3908,.F.);
#5692=ORIENTED_EDGE('',*,*,#3888,.T.);
#5693=ORIENTED_EDGE('',*,*,#3904,.T.);
#5694=ORIENTED_EDGE('',*,*,#3901,.T.);
#5695=ORIENTED_EDGE('',*,*,#3898,.T.);
#5696=ORIENTED_EDGE('',*,*,#3895,.T.);
#5697=ORIENTED_EDGE('',*,*,#3892,.T.);
#5698=ORIENTED_EDGE('',*,*,#3880,.T.);
#5699=ORIENTED_EDGE('',*,*,#3909,.F.);
#5700=ORIENTED_EDGE('',*,*,#3910,.T.);
#5701=ORIENTED_EDGE('',*,*,#3911,.T.);
#5702=ORIENTED_EDGE('',*,*,#3910,.F.);
#5703=ORIENTED_EDGE('',*,*,#3912,.F.);
#5704=ORIENTED_EDGE('',*,*,#3913,.T.);
#5705=ORIENTED_EDGE('',*,*,#3914,.T.);
#5706=ORIENTED_EDGE('',*,*,#3913,.F.);
#5707=ORIENTED_EDGE('',*,*,#3912,.T.);
#5708=ORIENTED_EDGE('',*,*,#3909,.T.);
#5709=ORIENTED_EDGE('',*,*,#3914,.F.);
#5710=ORIENTED_EDGE('',*,*,#3911,.F.);
#5711=ORIENTED_EDGE('',*,*,#3915,.T.);
#5712=ORIENTED_EDGE('',*,*,#3916,.T.);
#5713=ORIENTED_EDGE('',*,*,#3917,.F.);
#5714=ORIENTED_EDGE('',*,*,#3918,.T.);
#5715=ORIENTED_EDGE('',*,*,#3919,.T.);
#5716=ORIENTED_EDGE('',*,*,#3920,.T.);
#5717=ORIENTED_EDGE('',*,*,#3915,.F.);
#5718=ORIENTED_EDGE('',*,*,#3921,.T.);
#5719=ORIENTED_EDGE('',*,*,#3922,.T.);
#5720=ORIENTED_EDGE('',*,*,#3923,.T.);
#5721=ORIENTED_EDGE('',*,*,#3919,.F.);
#5722=ORIENTED_EDGE('',*,*,#3924,.T.);
#5723=ORIENTED_EDGE('',*,*,#3925,.T.);
#5724=ORIENTED_EDGE('',*,*,#3926,.T.);
#5725=ORIENTED_EDGE('',*,*,#3922,.F.);
#5726=ORIENTED_EDGE('',*,*,#3927,.T.);
#5727=ORIENTED_EDGE('',*,*,#3928,.F.);
#5728=ORIENTED_EDGE('',*,*,#3929,.T.);
#5729=ORIENTED_EDGE('',*,*,#3930,.F.);
#5730=ORIENTED_EDGE('',*,*,#3931,.T.);
#5731=ORIENTED_EDGE('',*,*,#3932,.T.);
#5732=ORIENTED_EDGE('',*,*,#3933,.T.);
#5733=ORIENTED_EDGE('',*,*,#3934,.F.);
#5734=ORIENTED_EDGE('',*,*,#3935,.F.);
#5735=ORIENTED_EDGE('',*,*,#3936,.T.);
#5736=ORIENTED_EDGE('',*,*,#3937,.T.);
#5737=ORIENTED_EDGE('',*,*,#3932,.F.);
#5738=ORIENTED_EDGE('',*,*,#3938,.F.);
#5739=ORIENTED_EDGE('',*,*,#3939,.T.);
#5740=ORIENTED_EDGE('',*,*,#3940,.T.);
#5741=ORIENTED_EDGE('',*,*,#3936,.F.);
#5742=ORIENTED_EDGE('',*,*,#3941,.F.);
#5743=ORIENTED_EDGE('',*,*,#3942,.T.);
#5744=ORIENTED_EDGE('',*,*,#3943,.T.);
#5745=ORIENTED_EDGE('',*,*,#3939,.F.);
#5746=ORIENTED_EDGE('',*,*,#3944,.F.);
#5747=ORIENTED_EDGE('',*,*,#3945,.F.);
#5748=ORIENTED_EDGE('',*,*,#3946,.F.);
#5749=ORIENTED_EDGE('',*,*,#3947,.F.);
#5750=ORIENTED_EDGE('',*,*,#3948,.T.);
#5751=ORIENTED_EDGE('',*,*,#3945,.T.);
#5752=ORIENTED_EDGE('',*,*,#3949,.T.);
#5753=ORIENTED_EDGE('',*,*,#3942,.F.);
#5754=ORIENTED_EDGE('',*,*,#3950,.F.);
#5755=ORIENTED_EDGE('',*,*,#3951,.F.);
#5756=ORIENTED_EDGE('',*,*,#3933,.F.);
#5757=ORIENTED_EDGE('',*,*,#3937,.F.);
#5758=ORIENTED_EDGE('',*,*,#3940,.F.);
#5759=ORIENTED_EDGE('',*,*,#3943,.F.);
#5760=ORIENTED_EDGE('',*,*,#3949,.F.);
#5761=ORIENTED_EDGE('',*,*,#3948,.F.);
#5762=ORIENTED_EDGE('',*,*,#3952,.F.);
#5763=ORIENTED_EDGE('',*,*,#3929,.F.);
#5764=ORIENTED_EDGE('',*,*,#3953,.F.);
#5765=ORIENTED_EDGE('',*,*,#3927,.F.);
#5766=ORIENTED_EDGE('',*,*,#3924,.F.);
#5767=ORIENTED_EDGE('',*,*,#3921,.F.);
#5768=ORIENTED_EDGE('',*,*,#3918,.F.);
#5769=ORIENTED_EDGE('',*,*,#3954,.F.);
#5770=ORIENTED_EDGE('',*,*,#3916,.F.);
#5771=ORIENTED_EDGE('',*,*,#3920,.F.);
#5772=ORIENTED_EDGE('',*,*,#3923,.F.);
#5773=ORIENTED_EDGE('',*,*,#3926,.F.);
#5774=ORIENTED_EDGE('',*,*,#3955,.F.);
#5775=ORIENTED_EDGE('',*,*,#3931,.F.);
#5776=ORIENTED_EDGE('',*,*,#3956,.F.);
#5777=ORIENTED_EDGE('',*,*,#3946,.T.);
#5778=ORIENTED_EDGE('',*,*,#3950,.T.);
#5779=ORIENTED_EDGE('',*,*,#3944,.T.);
#5780=ORIENTED_EDGE('',*,*,#3941,.T.);
#5781=ORIENTED_EDGE('',*,*,#3938,.T.);
#5782=ORIENTED_EDGE('',*,*,#3935,.T.);
#5783=ORIENTED_EDGE('',*,*,#3957,.T.);
#5784=ORIENTED_EDGE('',*,*,#3958,.T.);
#5785=ORIENTED_EDGE('',*,*,#3959,.T.);
#5786=ORIENTED_EDGE('',*,*,#3960,.T.);
#5787=ORIENTED_EDGE('',*,*,#3961,.T.);
#5788=ORIENTED_EDGE('',*,*,#3962,.T.);
#5789=ORIENTED_EDGE('',*,*,#3952,.T.);
#5790=ORIENTED_EDGE('',*,*,#3947,.T.);
#5791=ORIENTED_EDGE('',*,*,#3956,.T.);
#5792=ORIENTED_EDGE('',*,*,#3930,.T.);
#5793=ORIENTED_EDGE('',*,*,#3928,.T.);
#5794=ORIENTED_EDGE('',*,*,#3955,.T.);
#5795=ORIENTED_EDGE('',*,*,#3925,.F.);
#5796=ORIENTED_EDGE('',*,*,#3953,.T.);
#5797=ORIENTED_EDGE('',*,*,#3963,.T.);
#5798=ORIENTED_EDGE('',*,*,#3964,.T.);
#5799=ORIENTED_EDGE('',*,*,#3962,.F.);
#5800=ORIENTED_EDGE('',*,*,#3965,.F.);
#5801=ORIENTED_EDGE('',*,*,#3966,.T.);
#5802=ORIENTED_EDGE('',*,*,#3965,.T.);
#5803=ORIENTED_EDGE('',*,*,#3961,.F.);
#5804=ORIENTED_EDGE('',*,*,#3967,.F.);
#5805=ORIENTED_EDGE('',*,*,#3968,.T.);
#5806=ORIENTED_EDGE('',*,*,#3967,.T.);
#5807=ORIENTED_EDGE('',*,*,#3960,.F.);
#5808=ORIENTED_EDGE('',*,*,#3969,.F.);
#5809=ORIENTED_EDGE('',*,*,#3970,.T.);
#5810=ORIENTED_EDGE('',*,*,#3969,.T.);
#5811=ORIENTED_EDGE('',*,*,#3959,.F.);
#5812=ORIENTED_EDGE('',*,*,#3971,.F.);
#5813=ORIENTED_EDGE('',*,*,#3972,.T.);
#5814=ORIENTED_EDGE('',*,*,#3971,.T.);
#5815=ORIENTED_EDGE('',*,*,#3958,.F.);
#5816=ORIENTED_EDGE('',*,*,#3973,.F.);
#5817=ORIENTED_EDGE('',*,*,#3974,.T.);
#5818=ORIENTED_EDGE('',*,*,#3973,.T.);
#5819=ORIENTED_EDGE('',*,*,#3957,.F.);
#5820=ORIENTED_EDGE('',*,*,#3964,.F.);
#5821=ORIENTED_EDGE('',*,*,#3974,.F.);
#5822=ORIENTED_EDGE('',*,*,#3963,.F.);
#5823=ORIENTED_EDGE('',*,*,#3966,.F.);
#5824=ORIENTED_EDGE('',*,*,#3968,.F.);
#5825=ORIENTED_EDGE('',*,*,#3970,.F.);
#5826=ORIENTED_EDGE('',*,*,#3972,.F.);
#5827=ORIENTED_EDGE('',*,*,#3951,.T.);
#5828=ORIENTED_EDGE('',*,*,#3917,.T.);
#5829=ORIENTED_EDGE('',*,*,#3954,.T.);
#5830=ORIENTED_EDGE('',*,*,#3934,.T.);
#5831=CYLINDRICAL_SURFACE('',#6504,1.666);
#5832=CYLINDRICAL_SURFACE('',#6506,1.666);
#5833=CYLINDRICAL_SURFACE('',#6507,1.666);
#5834=CYLINDRICAL_SURFACE('',#6508,1.666);
#5835=CYLINDRICAL_SURFACE('',#6509,1.666);
#5836=CYLINDRICAL_SURFACE('',#6510,1.666);
#5837=CYLINDRICAL_SURFACE('',#6511,1.666);
#5838=CYLINDRICAL_SURFACE('',#6512,1.666);
#5839=CYLINDRICAL_SURFACE('',#6513,1.666);
#5840=CYLINDRICAL_SURFACE('',#6514,1.666);
#5841=CYLINDRICAL_SURFACE('',#6515,1.666);
#5842=CYLINDRICAL_SURFACE('',#6517,1.666);
#5843=CYLINDRICAL_SURFACE('',#6519,1.666);
#5844=CYLINDRICAL_SURFACE('',#6520,1.666);
#5845=CYLINDRICAL_SURFACE('',#6521,1.666);
#5846=CYLINDRICAL_SURFACE('',#6522,1.666);
#5847=CYLINDRICAL_SURFACE('',#6523,1.666);
#5848=CYLINDRICAL_SURFACE('',#6524,1.666);
#5849=CYLINDRICAL_SURFACE('',#6525,1.666);
#5850=CYLINDRICAL_SURFACE('',#6526,1.666);
#5851=CYLINDRICAL_SURFACE('',#6527,1.666);
#5852=CYLINDRICAL_SURFACE('',#6528,1.666);
#5853=CYLINDRICAL_SURFACE('',#6530,1.666);
#5854=CYLINDRICAL_SURFACE('',#6532,1.666);
#5855=CYLINDRICAL_SURFACE('',#6533,1.666);
#5856=CYLINDRICAL_SURFACE('',#6534,1.666);
#5857=CYLINDRICAL_SURFACE('',#6535,1.666);
#5858=CYLINDRICAL_SURFACE('',#6536,1.666);
#5859=CYLINDRICAL_SURFACE('',#6537,1.666);
#5860=CYLINDRICAL_SURFACE('',#6538,1.666);
#5861=CYLINDRICAL_SURFACE('',#6539,1.666);
#5862=CYLINDRICAL_SURFACE('',#6540,1.666);
#5863=CYLINDRICAL_SURFACE('',#6541,1.666);
#5864=CYLINDRICAL_SURFACE('',#6544,1.666);
#5865=CYLINDRICAL_SURFACE('',#6546,1.666);
#5866=CYLINDRICAL_SURFACE('',#6547,1.666);
#5867=CYLINDRICAL_SURFACE('',#6548,1.666);
#5868=CYLINDRICAL_SURFACE('',#6549,1.666);
#5869=CYLINDRICAL_SURFACE('',#6550,1.666);
#5870=CYLINDRICAL_SURFACE('',#6551,1.666);
#5871=CYLINDRICAL_SURFACE('',#6552,1.666);
#5872=CYLINDRICAL_SURFACE('',#6553,1.666);
#5873=CYLINDRICAL_SURFACE('',#6554,1.666);
#5874=CYLINDRICAL_SURFACE('',#6555,1.666);
#5875=CYLINDRICAL_SURFACE('',#6558,2.05475);
#5876=CYLINDRICAL_SURFACE('',#6560,2.05475);
#5877=CYLINDRICAL_SURFACE('',#6561,2.05475);
#5878=CYLINDRICAL_SURFACE('',#6562,2.05475);
#5879=CYLINDRICAL_SURFACE('',#6563,2.05475);
#5880=CYLINDRICAL_SURFACE('',#6564,2.05475);
#5881=CYLINDRICAL_SURFACE('',#6565,2.05475);
#5882=CYLINDRICAL_SURFACE('',#6566,2.05475);
#5883=CYLINDRICAL_SURFACE('',#6567,2.05475);
#5884=CYLINDRICAL_SURFACE('',#6568,2.05475);
#5885=CYLINDRICAL_SURFACE('',#6569,2.05475);
#5886=CYLINDRICAL_SURFACE('',#6570,2.05475);
#5887=CYLINDRICAL_SURFACE('',#6572,2.05475);
#5888=CYLINDRICAL_SURFACE('',#6574,2.05475);
#5889=CYLINDRICAL_SURFACE('',#6575,2.05475);
#5890=CYLINDRICAL_SURFACE('',#6576,2.05475);
#5891=CYLINDRICAL_SURFACE('',#6577,2.05475);
#5892=CYLINDRICAL_SURFACE('',#6578,2.05475);
#5893=CYLINDRICAL_SURFACE('',#6579,2.05475);
#5894=CYLINDRICAL_SURFACE('',#6580,2.05475);
#5895=CYLINDRICAL_SURFACE('',#6581,2.05475);
#5896=CYLINDRICAL_SURFACE('',#6582,2.05475);
#5897=CYLINDRICAL_SURFACE('',#6583,2.05475);
#5898=CYLINDRICAL_SURFACE('',#6584,2.05475);
#5899=CYLINDRICAL_SURFACE('',#6586,2.05475);
#5900=CYLINDRICAL_SURFACE('',#6588,2.05475);
#5901=CYLINDRICAL_SURFACE('',#6589,2.05475);
#5902=CYLINDRICAL_SURFACE('',#6590,2.05475);
#5903=CYLINDRICAL_SURFACE('',#6591,2.05475);
#5904=CYLINDRICAL_SURFACE('',#6592,2.05475);
#5905=CYLINDRICAL_SURFACE('',#6593,2.05475);
#5906=CYLINDRICAL_SURFACE('',#6594,2.05475);
#5907=CYLINDRICAL_SURFACE('',#6595,2.05475);
#5908=CYLINDRICAL_SURFACE('',#6596,2.05475);
#5909=CYLINDRICAL_SURFACE('',#6597,2.05475);
#5910=CYLINDRICAL_SURFACE('',#6598,2.05475);
#5911=CYLINDRICAL_SURFACE('',#6600,2.05475);
#5912=CYLINDRICAL_SURFACE('',#6602,2.05475);
#5913=CYLINDRICAL_SURFACE('',#6603,2.05475);
#5914=CYLINDRICAL_SURFACE('',#6604,2.05475);
#5915=CYLINDRICAL_SURFACE('',#6605,2.05475);
#5916=CYLINDRICAL_SURFACE('',#6606,2.05475);
#5917=CYLINDRICAL_SURFACE('',#6607,2.05475);
#5918=CYLINDRICAL_SURFACE('',#6608,2.05475);
#5919=CYLINDRICAL_SURFACE('',#6609,2.05475);
#5920=CYLINDRICAL_SURFACE('',#6610,2.05475);
#5921=CYLINDRICAL_SURFACE('',#6611,2.05475);
#5922=CYLINDRICAL_SURFACE('',#6612,2.05475);
#5923=CYLINDRICAL_SURFACE('',#6614,2.);
#5924=CYLINDRICAL_SURFACE('',#6617,2.);
#5925=CYLINDRICAL_SURFACE('',#6619,2.);
#5926=CYLINDRICAL_SURFACE('',#6621,2.);
#5927=CYLINDRICAL_SURFACE('',#6623,2.);
#5928=CYLINDRICAL_SURFACE('',#6625,2.);
#5929=CYLINDRICAL_SURFACE('',#6633,2.);
#5930=CYLINDRICAL_SURFACE('',#6636,2.);
#5931=CYLINDRICAL_SURFACE('',#6638,2.);
#5932=CYLINDRICAL_SURFACE('',#6640,2.);
#5933=CYLINDRICAL_SURFACE('',#6651,3.5);
#5934=CYLINDRICAL_SURFACE('',#6653,3.5);
#5935=CYLINDRICAL_SURFACE('',#6655,2.05475);
#5936=CYLINDRICAL_SURFACE('',#6657,2.05475);
#5937=CYLINDRICAL_SURFACE('',#6658,2.05475);
#5938=CYLINDRICAL_SURFACE('',#6659,2.05475);
#5939=CYLINDRICAL_SURFACE('',#6662,1.666);
#5940=CYLINDRICAL_SURFACE('',#6664,1.666);
#5941=CYLINDRICAL_SURFACE('',#6665,1.666);
#5942=CYLINDRICAL_SURFACE('',#6667,1.666);
#5943=CYLINDRICAL_SURFACE('',#6726,1.);
#5944=CYLINDRICAL_SURFACE('',#6727,1.);
#5945=CYLINDRICAL_SURFACE('',#6728,1.);
#5946=CYLINDRICAL_SURFACE('',#6729,1.);
#5947=CYLINDRICAL_SURFACE('',#6730,1.);
#5948=CYLINDRICAL_SURFACE('',#6731,1.);
#5949=CYLINDRICAL_SURFACE('',#6732,1.);
#5950=CYLINDRICAL_SURFACE('',#6733,1.);
#5951=CYLINDRICAL_SURFACE('',#6734,1.);
#5952=CYLINDRICAL_SURFACE('',#6735,1.);
#5953=CYLINDRICAL_SURFACE('',#6736,1.);
#5954=CYLINDRICAL_SURFACE('',#6737,1.);
#5955=CYLINDRICAL_SURFACE('',#6748,3.5);
#5956=CYLINDRICAL_SURFACE('',#6749,3.5);
#5957=CYLINDRICAL_SURFACE('',#6755,3.5);
#5958=CYLINDRICAL_SURFACE('',#6758,3.5);
#5959=CYLINDRICAL_SURFACE('',#6772,2.5);
#5960=CYLINDRICAL_SURFACE('',#6775,2.5);
#5961=CYLINDRICAL_SURFACE('',#6778,2.5);
#5962=CYLINDRICAL_SURFACE('',#6781,2.5);
#5963=CYLINDRICAL_SURFACE('',#6803,1.);
#5964=CYLINDRICAL_SURFACE('',#6813,1.);
#5965=CYLINDRICAL_SURFACE('',#6823,1.954);
#5966=CYLINDRICAL_SURFACE('',#6825,1.954);
#5967=CYLINDRICAL_SURFACE('',#6826,1.954);
#5968=CYLINDRICAL_SURFACE('',#6827,1.954);
#5969=CYLINDRICAL_SURFACE('',#6828,1.954);
#5970=CYLINDRICAL_SURFACE('',#6829,1.954);
#5971=CYLINDRICAL_SURFACE('',#6830,1.954);
#5972=CYLINDRICAL_SURFACE('',#6831,1.954);
#5973=CYLINDRICAL_SURFACE('',#6832,1.954);
#5974=CYLINDRICAL_SURFACE('',#6833,1.954);
#5975=CYLINDRICAL_SURFACE('',#6834,1.5555);
#5976=CYLINDRICAL_SURFACE('',#6836,1.5555);
#5977=CYLINDRICAL_SURFACE('',#6837,1.5555);
#5978=CYLINDRICAL_SURFACE('',#6838,1.5555);
#5979=CYLINDRICAL_SURFACE('',#6839,1.5555);
#5980=CYLINDRICAL_SURFACE('',#6840,1.5555);
#5981=CYLINDRICAL_SURFACE('',#6841,1.5555);
#5982=CYLINDRICAL_SURFACE('',#6842,1.5555);
#5983=CYLINDRICAL_SURFACE('',#6843,1.5555);
#5984=CYLINDRICAL_SURFACE('',#6844,1.5555);
#5985=CYLINDRICAL_SURFACE('',#6848,1.5555);
#5986=CYLINDRICAL_SURFACE('',#6850,1.954);
#5987=CYLINDRICAL_SURFACE('',#6860,3.5);
#5988=CYLINDRICAL_SURFACE('',#6865,2.942);
#5989=CYLINDRICAL_SURFACE('',#6867,2.942);
#5990=CYLINDRICAL_SURFACE('',#6868,2.942);
#5991=CYLINDRICAL_SURFACE('',#6869,2.942);
#5992=CYLINDRICAL_SURFACE('',#6870,2.942);
#5993=CYLINDRICAL_SURFACE('',#6871,2.942);
#5994=CYLINDRICAL_SURFACE('',#6872,2.942);
#5995=CYLINDRICAL_SURFACE('',#6873,2.942);
#5996=CYLINDRICAL_SURFACE('',#6874,2.942);
#5997=CYLINDRICAL_SURFACE('',#6875,2.942);
#5998=CYLINDRICAL_SURFACE('',#6876,2.942);
#5999=CYLINDRICAL_SURFACE('',#6877,2.942);
#6000=CYLINDRICAL_SURFACE('',#6878,2.942);
#6001=CYLINDRICAL_SURFACE('',#6879,2.942);
#6002=CYLINDRICAL_SURFACE('',#6880,2.942);
#6003=CYLINDRICAL_SURFACE('',#6881,2.37175);
#6004=CYLINDRICAL_SURFACE('',#6883,2.37175);
#6005=CYLINDRICAL_SURFACE('',#6884,2.37175);
#6006=CYLINDRICAL_SURFACE('',#6885,2.37175);
#6007=CYLINDRICAL_SURFACE('',#6886,2.37175);
#6008=CYLINDRICAL_SURFACE('',#6887,2.37175);
#6009=CYLINDRICAL_SURFACE('',#6888,2.37175);
#6010=CYLINDRICAL_SURFACE('',#6889,2.37175);
#6011=CYLINDRICAL_SURFACE('',#6890,2.37175);
#6012=CYLINDRICAL_SURFACE('',#6891,2.37175);
#6013=CYLINDRICAL_SURFACE('',#6892,2.37175);
#6014=CYLINDRICAL_SURFACE('',#6893,2.37175);
#6015=CYLINDRICAL_SURFACE('',#6894,2.37175);
#6016=CYLINDRICAL_SURFACE('',#6895,2.37175);
#6017=CYLINDRICAL_SURFACE('',#6896,2.37175);
#6018=CYLINDRICAL_SURFACE('',#6900,2.37175);
#6019=CYLINDRICAL_SURFACE('',#6902,2.942);
#6020=CYLINDRICAL_SURFACE('',#6912,5.);
#6021=CYLINDRICAL_SURFACE('',#6917,3.5);
#6022=CYLINDRICAL_SURFACE('',#6920,7.);
#6023=CYLINDRICAL_SURFACE('',#6926,2.5175);
#6024=CYLINDRICAL_SURFACE('',#6928,2.5175);
#6025=CYLINDRICAL_SURFACE('',#6929,2.5175);
#6026=CYLINDRICAL_SURFACE('',#6930,2.5175);
#6027=CYLINDRICAL_SURFACE('',#6931,2.5175);
#6028=CYLINDRICAL_SURFACE('',#6933,3.0735);
#6029=CYLINDRICAL_SURFACE('',#6935,3.0735);
#6030=CYLINDRICAL_SURFACE('',#6936,3.0735);
#6031=CYLINDRICAL_SURFACE('',#6937,3.0735);
#6032=CYLINDRICAL_SURFACE('',#6938,3.0735);
#6033=CYLINDRICAL_SURFACE('',#6940,3.0735);
#6034=CYLINDRICAL_SURFACE('',#6942,2.5175);
#6035=ADVANCED_FACE('',(#323),#5831,.F.);
#6036=ADVANCED_FACE('',(#324),#5832,.F.);
#6037=ADVANCED_FACE('',(#325),#5833,.F.);
#6038=ADVANCED_FACE('',(#326),#5834,.F.);
#6039=ADVANCED_FACE('',(#327),#5835,.F.);
#6040=ADVANCED_FACE('',(#328),#5836,.F.);
#6041=ADVANCED_FACE('',(#329),#5837,.F.);
#6042=ADVANCED_FACE('',(#330),#5838,.F.);
#6043=ADVANCED_FACE('',(#331),#5839,.F.);
#6044=ADVANCED_FACE('',(#332),#5840,.F.);
#6045=ADVANCED_FACE('',(#333),#5841,.F.);
#6046=ADVANCED_FACE('',(#334),#5842,.F.);
#6047=ADVANCED_FACE('',(#335),#5843,.F.);
#6048=ADVANCED_FACE('',(#336),#5844,.F.);
#6049=ADVANCED_FACE('',(#337),#5845,.F.);
#6050=ADVANCED_FACE('',(#338),#5846,.F.);
#6051=ADVANCED_FACE('',(#339),#5847,.F.);
#6052=ADVANCED_FACE('',(#340),#5848,.F.);
#6053=ADVANCED_FACE('',(#341),#5849,.F.);
#6054=ADVANCED_FACE('',(#342),#5850,.F.);
#6055=ADVANCED_FACE('',(#343),#5851,.F.);
#6056=ADVANCED_FACE('',(#344),#5852,.F.);
#6057=ADVANCED_FACE('',(#345),#5853,.F.);
#6058=ADVANCED_FACE('',(#346),#5854,.F.);
#6059=ADVANCED_FACE('',(#347),#5855,.F.);
#6060=ADVANCED_FACE('',(#348),#5856,.F.);
#6061=ADVANCED_FACE('',(#349),#5857,.F.);
#6062=ADVANCED_FACE('',(#350),#5858,.F.);
#6063=ADVANCED_FACE('',(#351),#5859,.F.);
#6064=ADVANCED_FACE('',(#352),#5860,.F.);
#6065=ADVANCED_FACE('',(#353),#5861,.F.);
#6066=ADVANCED_FACE('',(#354),#5862,.F.);
#6067=ADVANCED_FACE('',(#355),#5863,.F.);
#6068=ADVANCED_FACE('',(#356),#5864,.F.);
#6069=ADVANCED_FACE('',(#357),#5865,.F.);
#6070=ADVANCED_FACE('',(#358),#5866,.F.);
#6071=ADVANCED_FACE('',(#359),#5867,.F.);
#6072=ADVANCED_FACE('',(#360),#5868,.F.);
#6073=ADVANCED_FACE('',(#361),#5869,.F.);
#6074=ADVANCED_FACE('',(#362),#5870,.F.);
#6075=ADVANCED_FACE('',(#363),#5871,.F.);
#6076=ADVANCED_FACE('',(#364),#5872,.F.);
#6077=ADVANCED_FACE('',(#365),#5873,.F.);
#6078=ADVANCED_FACE('',(#366),#5874,.F.);
#6079=ADVANCED_FACE('',(#367),#5875,.F.);
#6080=ADVANCED_FACE('',(#368),#5876,.F.);
#6081=ADVANCED_FACE('',(#369),#5877,.F.);
#6082=ADVANCED_FACE('',(#370),#5878,.F.);
#6083=ADVANCED_FACE('',(#371),#5879,.F.);
#6084=ADVANCED_FACE('',(#372),#5880,.F.);
#6085=ADVANCED_FACE('',(#373),#5881,.F.);
#6086=ADVANCED_FACE('',(#374),#5882,.F.);
#6087=ADVANCED_FACE('',(#375),#5883,.F.);
#6088=ADVANCED_FACE('',(#376),#5884,.F.);
#6089=ADVANCED_FACE('',(#377),#5885,.F.);
#6090=ADVANCED_FACE('',(#378),#5886,.F.);
#6091=ADVANCED_FACE('',(#379),#5887,.F.);
#6092=ADVANCED_FACE('',(#380),#5888,.F.);
#6093=ADVANCED_FACE('',(#381),#5889,.F.);
#6094=ADVANCED_FACE('',(#382),#5890,.F.);
#6095=ADVANCED_FACE('',(#383),#5891,.F.);
#6096=ADVANCED_FACE('',(#384),#5892,.F.);
#6097=ADVANCED_FACE('',(#385),#5893,.F.);
#6098=ADVANCED_FACE('',(#386),#5894,.F.);
#6099=ADVANCED_FACE('',(#387),#5895,.F.);
#6100=ADVANCED_FACE('',(#388),#5896,.F.);
#6101=ADVANCED_FACE('',(#389),#5897,.F.);
#6102=ADVANCED_FACE('',(#390),#5898,.F.);
#6103=ADVANCED_FACE('',(#391),#5899,.F.);
#6104=ADVANCED_FACE('',(#392),#5900,.F.);
#6105=ADVANCED_FACE('',(#393),#5901,.F.);
#6106=ADVANCED_FACE('',(#394),#5902,.F.);
#6107=ADVANCED_FACE('',(#395),#5903,.F.);
#6108=ADVANCED_FACE('',(#396),#5904,.F.);
#6109=ADVANCED_FACE('',(#397),#5905,.F.);
#6110=ADVANCED_FACE('',(#398),#5906,.F.);
#6111=ADVANCED_FACE('',(#399),#5907,.F.);
#6112=ADVANCED_FACE('',(#400),#5908,.F.);
#6113=ADVANCED_FACE('',(#401),#5909,.F.);
#6114=ADVANCED_FACE('',(#402),#5910,.F.);
#6115=ADVANCED_FACE('',(#403),#5911,.F.);
#6116=ADVANCED_FACE('',(#404),#5912,.F.);
#6117=ADVANCED_FACE('',(#405),#5913,.F.);
#6118=ADVANCED_FACE('',(#406),#5914,.F.);
#6119=ADVANCED_FACE('',(#407),#5915,.F.);
#6120=ADVANCED_FACE('',(#408),#5916,.F.);
#6121=ADVANCED_FACE('',(#409),#5917,.F.);
#6122=ADVANCED_FACE('',(#410),#5918,.F.);
#6123=ADVANCED_FACE('',(#411),#5919,.F.);
#6124=ADVANCED_FACE('',(#412),#5920,.F.);
#6125=ADVANCED_FACE('',(#413),#5921,.F.);
#6126=ADVANCED_FACE('',(#414),#5922,.F.);
#6127=ADVANCED_FACE('',(#415),#5923,.T.);
#6128=ADVANCED_FACE('',(#416),#5924,.T.);
#6129=ADVANCED_FACE('',(#417),#5925,.T.);
#6130=ADVANCED_FACE('',(#418),#5926,.T.);
#6131=ADVANCED_FACE('',(#419),#5927,.T.);
#6132=ADVANCED_FACE('',(#420),#5928,.T.);
#6133=ADVANCED_FACE('',(#421),#197,.T.);
#6134=ADVANCED_FACE('',(#422),#198,.T.);
#6135=ADVANCED_FACE('',(#423),#199,.T.);
#6136=ADVANCED_FACE('',(#424,#145),#200,.T.);
#6137=ADVANCED_FACE('',(#425),#5929,.T.);
#6138=ADVANCED_FACE('',(#426),#5930,.T.);
#6139=ADVANCED_FACE('',(#427),#5931,.T.);
#6140=ADVANCED_FACE('',(#428),#5932,.T.);
#6141=ADVANCED_FACE('',(#429),#201,.T.);
#6142=ADVANCED_FACE('',(#430),#202,.T.);
#6143=ADVANCED_FACE('',(#431),#143,.T.);
#6144=ADVANCED_FACE('',(#432),#144,.T.);
#6145=ADVANCED_FACE('',(#433),#5933,.F.);
#6146=ADVANCED_FACE('',(#434),#5934,.F.);
#6147=ADVANCED_FACE('',(#435),#5935,.F.);
#6148=ADVANCED_FACE('',(#436),#129,.F.);
#6149=ADVANCED_FACE('',(#437),#130,.F.);
#6150=ADVANCED_FACE('',(#438,#146,#147,#148,#149,#150,#151,#152),#203,.F.);
#6151=ADVANCED_FACE('',(#439),#5936,.F.);
#6152=ADVANCED_FACE('',(#440),#131,.F.);
#6153=ADVANCED_FACE('',(#441),#132,.F.);
#6154=ADVANCED_FACE('',(#442),#5937,.F.);
#6155=ADVANCED_FACE('',(#443),#133,.F.);
#6156=ADVANCED_FACE('',(#444),#134,.F.);
#6157=ADVANCED_FACE('',(#445),#5938,.F.);
#6158=ADVANCED_FACE('',(#446),#135,.F.);
#6159=ADVANCED_FACE('',(#447),#136,.F.);
#6160=ADVANCED_FACE('',(#448,#153,#154,#155),#204,.T.);
#6161=ADVANCED_FACE('',(#449),#205,.F.);
#6162=ADVANCED_FACE('',(#450),#5939,.F.);
#6163=ADVANCED_FACE('',(#451),#206,.F.);
#6164=ADVANCED_FACE('',(#452),#5940,.F.);
#6165=ADVANCED_FACE('',(#453),#5941,.F.);
#6166=ADVANCED_FACE('',(#454),#207,.F.);
#6167=ADVANCED_FACE('',(#455),#5942,.F.);
#6168=ADVANCED_FACE('',(#456),#208,.F.);
#6169=ADVANCED_FACE('',(#457),#209,.F.);
#6170=ADVANCED_FACE('',(#458),#210,.F.);
#6171=ADVANCED_FACE('',(#459),#211,.F.);
#6172=ADVANCED_FACE('',(#460),#212,.F.);
#6173=ADVANCED_FACE('',(#461),#213,.F.);
#6174=ADVANCED_FACE('',(#462),#214,.F.);
#6175=ADVANCED_FACE('',(#463),#215,.F.);
#6176=ADVANCED_FACE('',(#464),#216,.F.);
#6177=ADVANCED_FACE('',(#465),#217,.F.);
#6178=ADVANCED_FACE('',(#466),#218,.F.);
#6179=ADVANCED_FACE('',(#467),#219,.F.);
#6180=ADVANCED_FACE('',(#468),#220,.F.);
#6181=ADVANCED_FACE('',(#469,#156,#157,#158),#221,.F.);
#6182=ADVANCED_FACE('',(#470),#222,.T.);
#6183=ADVANCED_FACE('',(#471),#223,.T.);
#6184=ADVANCED_FACE('',(#472),#224,.T.);
#6185=ADVANCED_FACE('',(#473),#225,.T.);
#6186=ADVANCED_FACE('',(#474),#226,.T.);
#6187=ADVANCED_FACE('',(#475),#227,.T.);
#6188=ADVANCED_FACE('',(#476),#228,.T.);
#6189=ADVANCED_FACE('',(#477),#229,.T.);
#6190=ADVANCED_FACE('',(#478),#230,.T.);
#6191=ADVANCED_FACE('',(#479),#231,.T.);
#6192=ADVANCED_FACE('',(#480),#232,.T.);
#6193=ADVANCED_FACE('',(#481),#81,.T.);
#6194=ADVANCED_FACE('',(#482),#82,.T.);
#6195=ADVANCED_FACE('',(#483),#83,.T.);
#6196=ADVANCED_FACE('',(#484),#84,.T.);
#6197=ADVANCED_FACE('',(#485),#85,.T.);
#6198=ADVANCED_FACE('',(#486),#86,.T.);
#6199=ADVANCED_FACE('',(#487),#87,.T.);
#6200=ADVANCED_FACE('',(#488),#88,.T.);
#6201=ADVANCED_FACE('',(#489),#5943,.T.);
#6202=ADVANCED_FACE('',(#490),#5944,.T.);
#6203=ADVANCED_FACE('',(#491),#5945,.T.);
#6204=ADVANCED_FACE('',(#492),#5946,.T.);
#6205=ADVANCED_FACE('',(#493),#5947,.T.);
#6206=ADVANCED_FACE('',(#494),#5948,.T.);
#6207=ADVANCED_FACE('',(#495),#5949,.T.);
#6208=ADVANCED_FACE('',(#496),#5950,.T.);
#6209=ADVANCED_FACE('',(#497),#5951,.T.);
#6210=ADVANCED_FACE('',(#498),#5952,.T.);
#6211=ADVANCED_FACE('',(#499),#5953,.T.);
#6212=ADVANCED_FACE('',(#500),#5954,.T.);
#6213=ADVANCED_FACE('',(#501),#233,.T.);
#6214=ADVANCED_FACE('',(#502,#159,#160,#161),#234,.F.);
#6215=ADVANCED_FACE('',(#503),#235,.T.);
#6216=ADVANCED_FACE('',(#504),#236,.T.);
#6217=ADVANCED_FACE('',(#505,#162,#163,#164),#237,.T.);
#6218=ADVANCED_FACE('',(#506),#238,.T.);
#6219=ADVANCED_FACE('',(#507),#5955,.F.);
#6220=ADVANCED_FACE('',(#508),#5956,.F.);
#6221=ADVANCED_FACE('',(#509),#239,.F.);
#6222=ADVANCED_FACE('',(#510),#240,.F.);
#6223=ADVANCED_FACE('',(#511),#241,.F.);
#6224=ADVANCED_FACE('',(#512),#242,.F.);
#6225=ADVANCED_FACE('',(#513),#5957,.F.);
#6226=ADVANCED_FACE('',(#514),#5958,.F.);
#6227=ADVANCED_FACE('',(#515),#243,.T.);
#6228=ADVANCED_FACE('',(#516),#244,.T.);
#6229=ADVANCED_FACE('',(#517),#245,.T.);
#6230=ADVANCED_FACE('',(#518),#246,.T.);
#6231=ADVANCED_FACE('',(#519),#247,.T.);
#6232=ADVANCED_FACE('',(#520),#248,.T.);
#6233=ADVANCED_FACE('',(#521),#249,.T.);
#6234=ADVANCED_FACE('',(#522),#250,.T.);
#6235=ADVANCED_FACE('',(#523,#165,#166,#167),#251,.T.);
#6236=ADVANCED_FACE('',(#524,#168,#169,#170),#252,.F.);
#6237=ADVANCED_FACE('',(#525),#5959,.F.);
#6238=ADVANCED_FACE('',(#526),#5960,.F.);
#6239=ADVANCED_FACE('',(#527),#5961,.F.);
#6240=ADVANCED_FACE('',(#528),#5962,.F.);
#6241=ADVANCED_FACE('',(#529),#253,.F.);
#6242=ADVANCED_FACE('',(#530),#254,.F.);
#6243=ADVANCED_FACE('',(#531),#255,.F.);
#6244=ADVANCED_FACE('',(#532),#256,.F.);
#6245=ADVANCED_FACE('',(#533),#257,.F.);
#6246=ADVANCED_FACE('',(#534),#258,.F.);
#6247=ADVANCED_FACE('',(#535),#259,.F.);
#6248=ADVANCED_FACE('',(#536),#260,.F.);
#6249=ADVANCED_FACE('',(#537),#261,.F.);
#6250=ADVANCED_FACE('',(#538),#262,.F.);
#6251=ADVANCED_FACE('',(#539),#263,.F.);
#6252=ADVANCED_FACE('',(#540),#264,.F.);
#6253=ADVANCED_FACE('',(#541),#265,.T.);
#6254=ADVANCED_FACE('',(#542),#266,.T.);
#6255=ADVANCED_FACE('',(#543),#267,.T.);
#6256=ADVANCED_FACE('',(#544),#268,.T.);
#6257=ADVANCED_FACE('',(#545,#171,#172,#173,#174,#175,#176,#177),#269,.T.);
#6258=ADVANCED_FACE('',(#546,#178,#179,#180,#181,#182,#183,#184),#270,.F.);
#6259=ADVANCED_FACE('',(#547),#5963,.F.);
#6260=ADVANCED_FACE('',(#548,#185),#271,.T.);
#6261=ADVANCED_FACE('',(#549),#272,.T.);
#6262=ADVANCED_FACE('',(#550,#186),#273,.T.);
#6263=ADVANCED_FACE('',(#551),#274,.T.);
#6264=ADVANCED_FACE('',(#552),#275,.T.);
#6265=ADVANCED_FACE('',(#553),#276,.F.);
#6266=ADVANCED_FACE('',(#554),#5964,.F.);
#6267=ADVANCED_FACE('',(#555,#187),#277,.T.);
#6268=ADVANCED_FACE('',(#556),#278,.T.);
#6269=ADVANCED_FACE('',(#557,#188),#279,.T.);
#6270=ADVANCED_FACE('',(#558),#280,.T.);
#6271=ADVANCED_FACE('',(#559),#281,.T.);
#6272=ADVANCED_FACE('',(#560),#282,.F.);
#6273=ADVANCED_FACE('',(#561),#5965,.T.);
#6274=ADVANCED_FACE('',(#562),#5966,.T.);
#6275=ADVANCED_FACE('',(#563),#5967,.T.);
#6276=ADVANCED_FACE('',(#564),#5968,.T.);
#6277=ADVANCED_FACE('',(#565),#5969,.T.);
#6278=ADVANCED_FACE('',(#566),#5970,.T.);
#6279=ADVANCED_FACE('',(#567),#5971,.T.);
#6280=ADVANCED_FACE('',(#568),#5972,.T.);
#6281=ADVANCED_FACE('',(#569),#5973,.T.);
#6282=ADVANCED_FACE('',(#570),#5974,.T.);
#6283=ADVANCED_FACE('',(#571),#5975,.T.);
#6284=ADVANCED_FACE('',(#572),#5976,.T.);
#6285=ADVANCED_FACE('',(#573),#5977,.T.);
#6286=ADVANCED_FACE('',(#574),#5978,.T.);
#6287=ADVANCED_FACE('',(#575),#5979,.T.);
#6288=ADVANCED_FACE('',(#576),#5980,.T.);
#6289=ADVANCED_FACE('',(#577),#5981,.T.);
#6290=ADVANCED_FACE('',(#578),#5982,.T.);
#6291=ADVANCED_FACE('',(#579),#5983,.T.);
#6292=ADVANCED_FACE('',(#580),#5984,.T.);
#6293=ADVANCED_FACE('',(#581),#79,.T.);
#6294=ADVANCED_FACE('',(#582),#137,.F.);
#6295=ADVANCED_FACE('',(#583),#5985,.T.);
#6296=ADVANCED_FACE('',(#584),#138,.F.);
#6297=ADVANCED_FACE('',(#585),#5986,.T.);
#6298=ADVANCED_FACE('',(#586),#283,.F.);
#6299=ADVANCED_FACE('',(#587),#284,.F.);
#6300=ADVANCED_FACE('',(#588),#285,.F.);
#6301=ADVANCED_FACE('',(#589),#286,.F.);
#6302=ADVANCED_FACE('',(#590),#287,.F.);
#6303=ADVANCED_FACE('',(#591),#288,.F.);
#6304=ADVANCED_FACE('',(#592),#289,.F.);
#6305=ADVANCED_FACE('',(#593,#189),#290,.T.);
#6306=ADVANCED_FACE('',(#594),#5987,.T.);
#6307=ADVANCED_FACE('',(#595,#190),#291,.F.);
#6308=ADVANCED_FACE('',(#596),#292,.T.);
#6309=ADVANCED_FACE('',(#597),#5988,.T.);
#6310=ADVANCED_FACE('',(#598),#5989,.T.);
#6311=ADVANCED_FACE('',(#599),#5990,.T.);
#6312=ADVANCED_FACE('',(#600),#5991,.T.);
#6313=ADVANCED_FACE('',(#601),#5992,.T.);
#6314=ADVANCED_FACE('',(#602),#5993,.T.);
#6315=ADVANCED_FACE('',(#603),#5994,.T.);
#6316=ADVANCED_FACE('',(#604),#5995,.T.);
#6317=ADVANCED_FACE('',(#605),#5996,.T.);
#6318=ADVANCED_FACE('',(#606),#5997,.T.);
#6319=ADVANCED_FACE('',(#607),#5998,.T.);
#6320=ADVANCED_FACE('',(#608),#5999,.T.);
#6321=ADVANCED_FACE('',(#609),#6000,.T.);
#6322=ADVANCED_FACE('',(#610),#6001,.T.);
#6323=ADVANCED_FACE('',(#611),#6002,.T.);
#6324=ADVANCED_FACE('',(#612),#6003,.T.);
#6325=ADVANCED_FACE('',(#613),#6004,.T.);
#6326=ADVANCED_FACE('',(#614),#6005,.T.);
#6327=ADVANCED_FACE('',(#615),#6006,.T.);
#6328=ADVANCED_FACE('',(#616),#6007,.T.);
#6329=ADVANCED_FACE('',(#617),#6008,.T.);
#6330=ADVANCED_FACE('',(#618),#6009,.T.);
#6331=ADVANCED_FACE('',(#619),#6010,.T.);
#6332=ADVANCED_FACE('',(#620),#6011,.T.);
#6333=ADVANCED_FACE('',(#621),#6012,.T.);
#6334=ADVANCED_FACE('',(#622),#6013,.T.);
#6335=ADVANCED_FACE('',(#623),#6014,.T.);
#6336=ADVANCED_FACE('',(#624),#6015,.T.);
#6337=ADVANCED_FACE('',(#625),#6016,.T.);
#6338=ADVANCED_FACE('',(#626),#6017,.T.);
#6339=ADVANCED_FACE('',(#627),#80,.T.);
#6340=ADVANCED_FACE('',(#628),#139,.F.);
#6341=ADVANCED_FACE('',(#629),#6018,.T.);
#6342=ADVANCED_FACE('',(#630),#140,.F.);
#6343=ADVANCED_FACE('',(#631),#6019,.T.);
#6344=ADVANCED_FACE('',(#632),#293,.F.);
#6345=ADVANCED_FACE('',(#633),#294,.F.);
#6346=ADVANCED_FACE('',(#634),#295,.F.);
#6347=ADVANCED_FACE('',(#635),#296,.F.);
#6348=ADVANCED_FACE('',(#636),#297,.F.);
#6349=ADVANCED_FACE('',(#637),#298,.F.);
#6350=ADVANCED_FACE('',(#638),#299,.F.);
#6351=ADVANCED_FACE('',(#639,#191),#300,.T.);
#6352=ADVANCED_FACE('',(#640),#6020,.T.);
#6353=ADVANCED_FACE('',(#641,#192),#301,.F.);
#6354=ADVANCED_FACE('',(#642),#302,.T.);
#6355=ADVANCED_FACE('',(#643),#6021,.F.);
#6356=ADVANCED_FACE('',(#644),#6022,.T.);
#6357=ADVANCED_FACE('',(#645,#193),#303,.T.);
#6358=ADVANCED_FACE('',(#646,#194),#304,.F.);
#6359=ADVANCED_FACE('',(#647),#6023,.F.);
#6360=ADVANCED_FACE('',(#648),#6024,.F.);
#6361=ADVANCED_FACE('',(#649),#6025,.F.);
#6362=ADVANCED_FACE('',(#650),#6026,.F.);
#6363=ADVANCED_FACE('',(#651),#6027,.F.);
#6364=ADVANCED_FACE('',(#652),#6028,.F.);
#6365=ADVANCED_FACE('',(#653),#6029,.F.);
#6366=ADVANCED_FACE('',(#654),#6030,.F.);
#6367=ADVANCED_FACE('',(#655),#6031,.F.);
#6368=ADVANCED_FACE('',(#656),#6032,.F.);
#6369=ADVANCED_FACE('',(#657),#6033,.F.);
#6370=ADVANCED_FACE('',(#658),#141,.F.);
#6371=ADVANCED_FACE('',(#659),#142,.F.);
#6372=ADVANCED_FACE('',(#660,#195),#305,.T.);
#6373=ADVANCED_FACE('',(#661),#6034,.F.);
#6374=ADVANCED_FACE('',(#662),#306,.T.);
#6375=ADVANCED_FACE('',(#663),#307,.T.);
#6376=ADVANCED_FACE('',(#664),#308,.T.);
#6377=ADVANCED_FACE('',(#665),#309,.T.);
#6378=ADVANCED_FACE('',(#666),#310,.T.);
#6379=ADVANCED_FACE('',(#667),#311,.T.);
#6380=ADVANCED_FACE('',(#668,#196),#312,.F.);
#6381=CLOSED_SHELL('',(#6035,#6036,#6037,#6038,#6039,#6040,#6041,#6042,
#6043,#6044,#6045,#6046,#6047,#6048,#6049,#6050,#6051,#6052,#6053,#6054,
#6055,#6056,#6057,#6058,#6059,#6060,#6061,#6062,#6063,#6064,#6065,#6066,
#6067,#6068,#6069,#6070,#6071,#6072,#6073,#6074,#6075,#6076,#6077,#6078,
#6079,#6080,#6081,#6082,#6083,#6084,#6085,#6086,#6087,#6088,#6089,#6090,
#6091,#6092,#6093,#6094,#6095,#6096,#6097,#6098,#6099,#6100,#6101,#6102,
#6103,#6104,#6105,#6106,#6107,#6108,#6109,#6110,#6111,#6112,#6113,#6114,
#6115,#6116,#6117,#6118,#6119,#6120,#6121,#6122,#6123,#6124,#6125,#6126,
#6127,#6128,#6129,#6130,#6131,#6132,#6133,#6134,#6135,#6136,#6137,#6138,
#6139,#6140,#6141,#6142,#6143,#6144,#6145,#6146,#6147,#6148,#6149,#6150,
#6151,#6152,#6153,#6154,#6155,#6156,#6157,#6158,#6159,#6160,#6161,#6162,
#6163,#6164,#6165,#6166,#6167,#6168,#6169,#6170,#6171,#6172,#6173,#6174,
#6175,#6176,#6177,#6178,#6179,#6180,#6181,#6182,#6183,#6184,#6185,#6186,
#6187,#6188,#6189,#6190,#6191,#6192));
#6382=CLOSED_SHELL('',(#6193,#6194,#6195,#6196,#6197,#6198,#6199,#6200,
#6201,#6202,#6203,#6204,#6205,#6206,#6207,#6208,#6209,#6210,#6211,#6212,
#6213,#6214,#6215,#6216,#6217,#6218,#6219,#6220,#6221,#6222,#6223,#6224));
#6383=CLOSED_SHELL('',(#6225,#6226,#6227,#6228,#6229,#6230,#6231,#6232,
#6233,#6234,#6235,#6236));
#6384=CLOSED_SHELL('',(#6237,#6238,#6239,#6240,#6241,#6242,#6243,#6244,
#6245,#6246,#6247,#6248,#6249,#6250,#6251,#6252,#6253,#6254,#6255,#6256,
#6257,#6258));
#6385=CLOSED_SHELL('',(#6259,#6260,#6261,#6262,#6263,#6264,#6265));
#6386=CLOSED_SHELL('',(#6266,#6267,#6268,#6269,#6270,#6271,#6272));
#6387=CLOSED_SHELL('',(#6273,#6274,#6275,#6276,#6277,#6278,#6279,#6280,
#6281,#6282,#6283,#6284,#6285,#6286,#6287,#6288,#6289,#6290,#6291,#6292,
#6293,#6294,#6295,#6296,#6297,#6298,#6299,#6300,#6301,#6302,#6303,#6304,
#6305,#6306,#6307,#6308));
#6388=CLOSED_SHELL('',(#6309,#6310,#6311,#6312,#6313,#6314,#6315,#6316,
#6317,#6318,#6319,#6320,#6321,#6322,#6323,#6324,#6325,#6326,#6327,#6328,
#6329,#6330,#6331,#6332,#6333,#6334,#6335,#6336,#6337,#6338,#6339,#6340,
#6341,#6342,#6343,#6344,#6345,#6346,#6347,#6348,#6349,#6350,#6351,#6352,
#6353,#6354));
#6389=CLOSED_SHELL('',(#6355,#6356,#6357,#6358));
#6390=CLOSED_SHELL('',(#6359,#6360,#6361,#6362,#6363,#6364,#6365,#6366,
#6367,#6368,#6369,#6370,#6371,#6372,#6373,#6374,#6375,#6376,#6377,#6378,
#6379,#6380));
#6391=DERIVED_UNIT_ELEMENT(#6411,1.);
#6392=DERIVED_UNIT_ELEMENT(#21882,-3.);
#6393=DERIVED_UNIT_ELEMENT(#6411,1.);
#6394=DERIVED_UNIT_ELEMENT(#21882,-3.);
#6395=DERIVED_UNIT_ELEMENT(#6411,1.);
#6396=DERIVED_UNIT_ELEMENT(#21882,-3.);
#6397=DERIVED_UNIT_ELEMENT(#6411,1.);
#6398=DERIVED_UNIT_ELEMENT(#21882,-3.);
#6399=DERIVED_UNIT_ELEMENT(#6411,1.);
#6400=DERIVED_UNIT_ELEMENT(#21882,-3.);
#6401=DERIVED_UNIT_ELEMENT(#6411,1.);
#6402=DERIVED_UNIT_ELEMENT(#21882,-3.);
#6403=DERIVED_UNIT_ELEMENT(#6411,1.);
#6404=DERIVED_UNIT_ELEMENT(#21882,-3.);
#6405=DERIVED_UNIT_ELEMENT(#6411,1.);
#6406=DERIVED_UNIT_ELEMENT(#21882,-3.);
#6407=DERIVED_UNIT_ELEMENT(#6411,1.);
#6408=DERIVED_UNIT_ELEMENT(#21882,-3.);
#6409=DERIVED_UNIT_ELEMENT(#6411,1.);
#6410=DERIVED_UNIT_ELEMENT(#21882,-3.);
#6411=(
MASS_UNIT()
NAMED_UNIT(*)
SI_UNIT(.KILO.,.GRAM.)
);
#6412=DERIVED_UNIT((#6391,#6392));
#6413=DERIVED_UNIT((#6393,#6394));
#6414=DERIVED_UNIT((#6395,#6396));
#6415=DERIVED_UNIT((#6397,#6398));
#6416=DERIVED_UNIT((#6399,#6400));
#6417=DERIVED_UNIT((#6401,#6402));
#6418=DERIVED_UNIT((#6403,#6404));
#6419=DERIVED_UNIT((#6405,#6406));
#6420=DERIVED_UNIT((#6407,#6408));
#6421=DERIVED_UNIT((#6409,#6410));
#6422=MEASURE_REPRESENTATION_ITEM('density measure',
POSITIVE_RATIO_MEASURE(1130.),#6412);
#6423=MEASURE_REPRESENTATION_ITEM('density measure',
POSITIVE_RATIO_MEASURE(7850.),#6413);
#6424=MEASURE_REPRESENTATION_ITEM('density measure',
POSITIVE_RATIO_MEASURE(1250.),#6414);
#6425=MEASURE_REPRESENTATION_ITEM('density measure',
POSITIVE_RATIO_MEASURE(1130.),#6415);
#6426=MEASURE_REPRESENTATION_ITEM('density measure',
POSITIVE_RATIO_MEASURE(8940.),#6416);
#6427=MEASURE_REPRESENTATION_ITEM('density measure',
POSITIVE_RATIO_MEASURE(8940.),#6417);
#6428=MEASURE_REPRESENTATION_ITEM('density measure',
POSITIVE_RATIO_MEASURE(7850.),#6418);
#6429=MEASURE_REPRESENTATION_ITEM('density measure',
POSITIVE_RATIO_MEASURE(7850.),#6419);
#6430=MEASURE_REPRESENTATION_ITEM('density measure',
POSITIVE_RATIO_MEASURE(7850.),#6420);
#6431=MEASURE_REPRESENTATION_ITEM('density measure',
POSITIVE_RATIO_MEASURE(7850.),#6421);
#6432=PROPERTY_DEFINITION_REPRESENTATION(#6482,#6452);
#6433=PROPERTY_DEFINITION_REPRESENTATION(#6483,#6453);
#6434=PROPERTY_DEFINITION_REPRESENTATION(#6484,#6454);
#6435=PROPERTY_DEFINITION_REPRESENTATION(#6485,#6455);
#6436=PROPERTY_DEFINITION_REPRESENTATION(#6486,#6456);
#6437=PROPERTY_DEFINITION_REPRESENTATION(#6487,#6457);
#6438=PROPERTY_DEFINITION_REPRESENTATION(#6488,#6458);
#6439=PROPERTY_DEFINITION_REPRESENTATION(#6489,#6459);
#6440=PROPERTY_DEFINITION_REPRESENTATION(#6490,#6460);
#6441=PROPERTY_DEFINITION_REPRESENTATION(#6491,#6461);
#6442=PROPERTY_DEFINITION_REPRESENTATION(#6492,#6462);
#6443=PROPERTY_DEFINITION_REPRESENTATION(#6493,#6463);
#6444=PROPERTY_DEFINITION_REPRESENTATION(#6494,#6464);
#6445=PROPERTY_DEFINITION_REPRESENTATION(#6495,#6465);
#6446=PROPERTY_DEFINITION_REPRESENTATION(#6496,#6466);
#6447=PROPERTY_DEFINITION_REPRESENTATION(#6497,#6467);
#6448=PROPERTY_DEFINITION_REPRESENTATION(#6498,#6468);
#6449=PROPERTY_DEFINITION_REPRESENTATION(#6499,#6469);
#6450=PROPERTY_DEFINITION_REPRESENTATION(#6500,#6470);
#6451=PROPERTY_DEFINITION_REPRESENTATION(#6501,#6471);
#6452=REPRESENTATION('material name',(#6472),#21870);
#6453=REPRESENTATION('density',(#6422),#21870);
#6454=REPRESENTATION('material name',(#6473),#21871);
#6455=REPRESENTATION('density',(#6423),#21871);
#6456=REPRESENTATION('material name',(#6474),#21872);
#6457=REPRESENTATION('density',(#6424),#21872);
#6458=REPRESENTATION('material name',(#6475),#21873);
#6459=REPRESENTATION('density',(#6425),#21873);
#6460=REPRESENTATION('material name',(#6476),#21874);
#6461=REPRESENTATION('density',(#6426),#21874);
#6462=REPRESENTATION('material name',(#6477),#21875);
#6463=REPRESENTATION('density',(#6427),#21875);
#6464=REPRESENTATION('material name',(#6478),#21876);
#6465=REPRESENTATION('density',(#6428),#21876);
#6466=REPRESENTATION('material name',(#6479),#21877);
#6467=REPRESENTATION('density',(#6429),#21877);
#6468=REPRESENTATION('material name',(#6480),#21878);
#6469=REPRESENTATION('density',(#6430),#21878);
#6470=REPRESENTATION('material name',(#6481),#21879);
#6471=REPRESENTATION('density',(#6431),#21879);
#6472=DESCRIPTIVE_REPRESENTATION_ITEM('Nylon 6/6','Nylon 6/6');
#6473=DESCRIPTIVE_REPRESENTATION_ITEM('Steel','Steel');
#6474=DESCRIPTIVE_REPRESENTATION_ITEM('Rubber, Silicone',
'Rubber, Silicone');
#6475=DESCRIPTIVE_REPRESENTATION_ITEM('Nylon 6/6','Nylon 6/6');
#6476=DESCRIPTIVE_REPRESENTATION_ITEM('Copper','Copper');
#6477=DESCRIPTIVE_REPRESENTATION_ITEM('Copper','Copper');
#6478=DESCRIPTIVE_REPRESENTATION_ITEM('Steel','Steel');
#6479=DESCRIPTIVE_REPRESENTATION_ITEM('Steel','Steel');
#6480=DESCRIPTIVE_REPRESENTATION_ITEM('Steel','Steel');
#6481=DESCRIPTIVE_REPRESENTATION_ITEM('Steel','Steel');
#6482=PROPERTY_DEFINITION('material property','material name',#21937);
#6483=PROPERTY_DEFINITION('material property','density of part',#21937);
#6484=PROPERTY_DEFINITION('material property','material name',#21938);
#6485=PROPERTY_DEFINITION('material property','density of part',#21938);
#6486=PROPERTY_DEFINITION('material property','material name',#21939);
#6487=PROPERTY_DEFINITION('material property','density of part',#21939);
#6488=PROPERTY_DEFINITION('material property','material name',#21940);
#6489=PROPERTY_DEFINITION('material property','density of part',#21940);
#6490=PROPERTY_DEFINITION('material property','material name',#21941);
#6491=PROPERTY_DEFINITION('material property','density of part',#21941);
#6492=PROPERTY_DEFINITION('material property','material name',#21942);
#6493=PROPERTY_DEFINITION('material property','density of part',#21942);
#6494=PROPERTY_DEFINITION('material property','material name',#21943);
#6495=PROPERTY_DEFINITION('material property','density of part',#21943);
#6496=PROPERTY_DEFINITION('material property','material name',#21944);
#6497=PROPERTY_DEFINITION('material property','density of part',#21944);
#6498=PROPERTY_DEFINITION('material property','material name',#21945);
#6499=PROPERTY_DEFINITION('material property','density of part',#21945);
#6500=PROPERTY_DEFINITION('material property','material name',#21946);
#6501=PROPERTY_DEFINITION('material property','density of part',#21946);
#6502=AXIS2_PLACEMENT_3D('',#8353,#6967,#6968);
#6503=AXIS2_PLACEMENT_3D('',#8354,#6969,#6970);
#6504=AXIS2_PLACEMENT_3D('',#8355,#6971,#6972);
#6505=AXIS2_PLACEMENT_3D('',#8374,#6974,#6975);
#6506=AXIS2_PLACEMENT_3D('',#8394,#6976,#6977);
#6507=AXIS2_PLACEMENT_3D('',#8442,#6979,#6980);
#6508=AXIS2_PLACEMENT_3D('',#8490,#6982,#6983);
#6509=AXIS2_PLACEMENT_3D('',#8541,#6985,#6986);
#6510=AXIS2_PLACEMENT_3D('',#8589,#6988,#6989);
#6511=AXIS2_PLACEMENT_3D('',#8637,#6991,#6992);
#6512=AXIS2_PLACEMENT_3D('',#8688,#6994,#6995);
#6513=AXIS2_PLACEMENT_3D('',#8739,#6997,#6998);
#6514=AXIS2_PLACEMENT_3D('',#8787,#7000,#7001);
#6515=AXIS2_PLACEMENT_3D('',#8838,#7003,#7004);
#6516=AXIS2_PLACEMENT_3D('',#8857,#7006,#7007);
#6517=AXIS2_PLACEMENT_3D('',#8877,#7008,#7009);
#6518=AXIS2_PLACEMENT_3D('',#8896,#7011,#7012);
#6519=AXIS2_PLACEMENT_3D('',#8916,#7013,#7014);
#6520=AXIS2_PLACEMENT_3D('',#8964,#7016,#7017);
#6521=AXIS2_PLACEMENT_3D('',#9012,#7019,#7020);
#6522=AXIS2_PLACEMENT_3D('',#9063,#7022,#7023);
#6523=AXIS2_PLACEMENT_3D('',#9111,#7025,#7026);
#6524=AXIS2_PLACEMENT_3D('',#9159,#7028,#7029);
#6525=AXIS2_PLACEMENT_3D('',#9210,#7031,#7032);
#6526=AXIS2_PLACEMENT_3D('',#9261,#7034,#7035);
#6527=AXIS2_PLACEMENT_3D('',#9309,#7037,#7038);
#6528=AXIS2_PLACEMENT_3D('',#9360,#7040,#7041);
#6529=AXIS2_PLACEMENT_3D('',#9379,#7043,#7044);
#6530=AXIS2_PLACEMENT_3D('',#9399,#7045,#7046);
#6531=AXIS2_PLACEMENT_3D('',#9418,#7048,#7049);
#6532=AXIS2_PLACEMENT_3D('',#9438,#7050,#7051);
#6533=AXIS2_PLACEMENT_3D('',#9486,#7053,#7054);
#6534=AXIS2_PLACEMENT_3D('',#9534,#7056,#7057);
#6535=AXIS2_PLACEMENT_3D('',#9585,#7059,#7060);
#6536=AXIS2_PLACEMENT_3D('',#9633,#7062,#7063);
#6537=AXIS2_PLACEMENT_3D('',#9681,#7065,#7066);
#6538=AXIS2_PLACEMENT_3D('',#9732,#7068,#7069);
#6539=AXIS2_PLACEMENT_3D('',#9783,#7071,#7072);
#6540=AXIS2_PLACEMENT_3D('',#9831,#7074,#7075);
#6541=AXIS2_PLACEMENT_3D('',#9882,#7077,#7078);
#6542=AXIS2_PLACEMENT_3D('',#9901,#7080,#7081);
#6543=AXIS2_PLACEMENT_3D('',#9903,#7082,#7083);
#6544=AXIS2_PLACEMENT_3D('',#9923,#7084,#7085);
#6545=AXIS2_PLACEMENT_3D('',#9942,#7087,#7088);
#6546=AXIS2_PLACEMENT_3D('',#9962,#7089,#7090);
#6547=AXIS2_PLACEMENT_3D('',#10010,#7092,#7093);
#6548=AXIS2_PLACEMENT_3D('',#10058,#7095,#7096);
#6549=AXIS2_PLACEMENT_3D('',#10109,#7098,#7099);
#6550=AXIS2_PLACEMENT_3D('',#10157,#7101,#7102);
#6551=AXIS2_PLACEMENT_3D('',#10205,#7104,#7105);
#6552=AXIS2_PLACEMENT_3D('',#10256,#7107,#7108);
#6553=AXIS2_PLACEMENT_3D('',#10307,#7110,#7111);
#6554=AXIS2_PLACEMENT_3D('',#10355,#7113,#7114);
#6555=AXIS2_PLACEMENT_3D('',#10406,#7116,#7117);
#6556=AXIS2_PLACEMENT_3D('',#10425,#7119,#7120);
#6557=AXIS2_PLACEMENT_3D('',#10427,#7121,#7122);
#6558=AXIS2_PLACEMENT_3D('',#10447,#7123,#7124);
#6559=AXIS2_PLACEMENT_3D('',#10457,#7126,#7127);
#6560=AXIS2_PLACEMENT_3D('',#10463,#7128,#7129);
#6561=AXIS2_PLACEMENT_3D('',#10488,#7131,#7132);
#6562=AXIS2_PLACEMENT_3D('',#10513,#7134,#7135);
#6563=AXIS2_PLACEMENT_3D('',#10537,#7137,#7138);
#6564=AXIS2_PLACEMENT_3D('',#10562,#7140,#7141);
#6565=AXIS2_PLACEMENT_3D('',#10586,#7143,#7144);
#6566=AXIS2_PLACEMENT_3D('',#10611,#7146,#7147);
#6567=AXIS2_PLACEMENT_3D('',#10635,#7149,#7150);
#6568=AXIS2_PLACEMENT_3D('',#10660,#7152,#7153);
#6569=AXIS2_PLACEMENT_3D('',#10685,#7155,#7156);
#6570=AXIS2_PLACEMENT_3D('',#10709,#7158,#7159);
#6571=AXIS2_PLACEMENT_3D('',#10720,#7161,#7162);
#6572=AXIS2_PLACEMENT_3D('',#10726,#7163,#7164);
#6573=AXIS2_PLACEMENT_3D('',#10736,#7166,#7167);
#6574=AXIS2_PLACEMENT_3D('',#10742,#7168,#7169);
#6575=AXIS2_PLACEMENT_3D('',#10767,#7171,#7172);
#6576=AXIS2_PLACEMENT_3D('',#10792,#7174,#7175);
#6577=AXIS2_PLACEMENT_3D('',#10816,#7177,#7178);
#6578=AXIS2_PLACEMENT_3D('',#10841,#7180,#7181);
#6579=AXIS2_PLACEMENT_3D('',#10865,#7183,#7184);
#6580=AXIS2_PLACEMENT_3D('',#10890,#7186,#7187);
#6581=AXIS2_PLACEMENT_3D('',#10914,#7189,#7190);
#6582=AXIS2_PLACEMENT_3D('',#10939,#7192,#7193);
#6583=AXIS2_PLACEMENT_3D('',#10964,#7195,#7196);
#6584=AXIS2_PLACEMENT_3D('',#10988,#7198,#7199);
#6585=AXIS2_PLACEMENT_3D('',#10999,#7201,#7202);
#6586=AXIS2_PLACEMENT_3D('',#11005,#7203,#7204);
#6587=AXIS2_PLACEMENT_3D('',#11015,#7206,#7207);
#6588=AXIS2_PLACEMENT_3D('',#11021,#7208,#7209);
#6589=AXIS2_PLACEMENT_3D('',#11046,#7211,#7212);
#6590=AXIS2_PLACEMENT_3D('',#11071,#7214,#7215);
#6591=AXIS2_PLACEMENT_3D('',#11095,#7217,#7218);
#6592=AXIS2_PLACEMENT_3D('',#11120,#7220,#7221);
#6593=AXIS2_PLACEMENT_3D('',#11144,#7223,#7224);
#6594=AXIS2_PLACEMENT_3D('',#11169,#7226,#7227);
#6595=AXIS2_PLACEMENT_3D('',#11193,#7229,#7230);
#6596=AXIS2_PLACEMENT_3D('',#11218,#7232,#7233);
#6597=AXIS2_PLACEMENT_3D('',#11243,#7235,#7236);
#6598=AXIS2_PLACEMENT_3D('',#11267,#7238,#7239);
#6599=AXIS2_PLACEMENT_3D('',#11278,#7241,#7242);
#6600=AXIS2_PLACEMENT_3D('',#11284,#7243,#7244);
#6601=AXIS2_PLACEMENT_3D('',#11294,#7246,#7247);
#6602=AXIS2_PLACEMENT_3D('',#11300,#7248,#7249);
#6603=AXIS2_PLACEMENT_3D('',#11325,#7251,#7252);
#6604=AXIS2_PLACEMENT_3D('',#11350,#7254,#7255);
#6605=AXIS2_PLACEMENT_3D('',#11374,#7257,#7258);
#6606=AXIS2_PLACEMENT_3D('',#11399,#7260,#7261);
#6607=AXIS2_PLACEMENT_3D('',#11423,#7263,#7264);
#6608=AXIS2_PLACEMENT_3D('',#11448,#7266,#7267);
#6609=AXIS2_PLACEMENT_3D('',#11472,#7269,#7270);
#6610=AXIS2_PLACEMENT_3D('',#11497,#7272,#7273);
#6611=AXIS2_PLACEMENT_3D('',#11522,#7275,#7276);
#6612=AXIS2_PLACEMENT_3D('',#11546,#7278,#7279);
#6613=AXIS2_PLACEMENT_3D('',#11557,#7281,#7282);
#6614=AXIS2_PLACEMENT_3D('',#11563,#7283,#7284);
#6615=AXIS2_PLACEMENT_3D('',#11568,#7286,#7287);
#6616=AXIS2_PLACEMENT_3D('',#11571,#7289,#7290);
#6617=AXIS2_PLACEMENT_3D('',#11572,#7291,#7292);
#6618=AXIS2_PLACEMENT_3D('',#11576,#7294,#7295);
#6619=AXIS2_PLACEMENT_3D('',#11578,#7297,#7298);
#6620=AXIS2_PLACEMENT_3D('',#11582,#7300,#7301);
#6621=AXIS2_PLACEMENT_3D('',#11584,#7303,#7304);
#6622=AXIS2_PLACEMENT_3D('',#11588,#7306,#7307);
#6623=AXIS2_PLACEMENT_3D('',#11590,#7309,#7310);
#6624=AXIS2_PLACEMENT_3D('',#11595,#7313,#7314);
#6625=AXIS2_PLACEMENT_3D('',#11596,#7315,#7316);
#6626=AXIS2_PLACEMENT_3D('',#11599,#7319,#7320);
#6627=AXIS2_PLACEMENT_3D('',#11609,#7326,#7327);
#6628=AXIS2_PLACEMENT_3D('',#11614,#7331,#7332);
#6629=AXIS2_PLACEMENT_3D('',#11618,#7335,#7336);
#6630=AXIS2_PLACEMENT_3D('',#11623,#7338,#7339);
#6631=AXIS2_PLACEMENT_3D('',#11631,#7343,#7344);
#6632=AXIS2_PLACEMENT_3D('',#11633,#7345,#7346);
#6633=AXIS2_PLACEMENT_3D('',#11637,#7349,#7350);
#6634=AXIS2_PLACEMENT_3D('',#11660,#7351,#7352);
#6635=AXIS2_PLACEMENT_3D('',#11663,#7354,#7355);
#6636=AXIS2_PLACEMENT_3D('',#11664,#7356,#7357);
#6637=AXIS2_PLACEMENT_3D('',#11666,#7358,#7359);
#6638=AXIS2_PLACEMENT_3D('',#11668,#7361,#7362);
#6639=AXIS2_PLACEMENT_3D('',#11688,#7363,#7364);
#6640=AXIS2_PLACEMENT_3D('',#11690,#7366,#7367);
#6641=AXIS2_PLACEMENT_3D('',#11692,#7369,#7370);
#6642=AXIS2_PLACEMENT_3D('',#11698,#7374,#7375);
#6643=AXIS2_PLACEMENT_3D('',#11702,#7378,#7379);
#6644=AXIS2_PLACEMENT_3D('',#11704,#7380,#7381);
#6645=AXIS2_PLACEMENT_3D('',#11706,#7382,#7383);
#6646=AXIS2_PLACEMENT_3D('',#11707,#7384,#7385);
#6647=AXIS2_PLACEMENT_3D('',#11708,#7386,#7387);
#6648=AXIS2_PLACEMENT_3D('',#11710,#7388,#7389);
#6649=AXIS2_PLACEMENT_3D('',#11712,#7390,#7391);
#6650=AXIS2_PLACEMENT_3D('',#11713,#7392,#7393);
#6651=AXIS2_PLACEMENT_3D('',#11714,#7394,#7395);
#6652=AXIS2_PLACEMENT_3D('',#11717,#7397,#7398);
#6653=AXIS2_PLACEMENT_3D('',#11718,#7399,#7400);
#6654=AXIS2_PLACEMENT_3D('',#11721,#7402,#7403);
#6655=AXIS2_PLACEMENT_3D('',#11722,#7404,#7405);
#6656=AXIS2_PLACEMENT_3D('',#12745,#7406,#7407);
#6657=AXIS2_PLACEMENT_3D('',#13283,#7426,#7427);
#6658=AXIS2_PLACEMENT_3D('',#14141,#7428,#7429);
#6659=AXIS2_PLACEMENT_3D('',#14999,#7430,#7431);
#6660=AXIS2_PLACEMENT_3D('',#15861,#7432,#7433);
#6661=AXIS2_PLACEMENT_3D('',#15891,#7449,#7450);
#6662=AXIS2_PLACEMENT_3D('',#15892,#7451,#7452);
#6663=AXIS2_PLACEMENT_3D('',#15893,#7453,#7454);
#6664=AXIS2_PLACEMENT_3D('',#15895,#7456,#7457);
#6665=AXIS2_PLACEMENT_3D('',#15896,#7458,#7459);
#6666=AXIS2_PLACEMENT_3D('',#15897,#7460,#7461);
#6667=AXIS2_PLACEMENT_3D('',#15898,#7462,#7463);
#6668=AXIS2_PLACEMENT_3D('',#15899,#7464,#7465);
#6669=AXIS2_PLACEMENT_3D('',#15900,#7466,#7467);
#6670=AXIS2_PLACEMENT_3D('',#15903,#7470,#7471);
#6671=AXIS2_PLACEMENT_3D('',#15905,#7473,#7474);
#6672=AXIS2_PLACEMENT_3D('',#15907,#7476,#7477);
#6673=AXIS2_PLACEMENT_3D('',#15908,#7478,#7479);
#6674=AXIS2_PLACEMENT_3D('',#15911,#7482,#7483);
#6675=AXIS2_PLACEMENT_3D('',#15913,#7485,#7486);
#6676=AXIS2_PLACEMENT_3D('',#15915,#7488,#7489);
#6677=AXIS2_PLACEMENT_3D('',#15916,#7490,#7491);
#6678=AXIS2_PLACEMENT_3D('',#15919,#7494,#7495);
#6679=AXIS2_PLACEMENT_3D('',#15921,#7497,#7498);
#6680=AXIS2_PLACEMENT_3D('',#15923,#7500,#7501);
#6681=AXIS2_PLACEMENT_3D('',#15924,#7502,#7503);
#6682=AXIS2_PLACEMENT_3D('',#15940,#7512,#7513);
#6683=AXIS2_PLACEMENT_3D('',#15942,#7515,#7516);
#6684=AXIS2_PLACEMENT_3D('',#15943,#7517,#7518);
#6685=AXIS2_PLACEMENT_3D('',#15945,#7520,#7521);
#6686=AXIS2_PLACEMENT_3D('',#15947,#7523,#7524);
#6687=AXIS2_PLACEMENT_3D('',#15950,#7527,#7528);
#6688=AXIS2_PLACEMENT_3D('',#15952,#7530,#7531);
#6689=AXIS2_PLACEMENT_3D('',#15954,#7533,#7534);
#6690=AXIS2_PLACEMENT_3D('',#15955,#7535,#7536);
#6691=AXIS2_PLACEMENT_3D('',#15957,#7538,#7539);
#6692=AXIS2_PLACEMENT_3D('',#15959,#7541,#7542);
#6693=AXIS2_PLACEMENT_3D('',#15960,#7543,#7544);
#6694=AXIS2_PLACEMENT_3D('',#15961,#7545,#7546);
#6695=AXIS2_PLACEMENT_3D('',#15964,#7547,#7548);
#6696=AXIS2_PLACEMENT_3D('',#15966,#7549,#7550);
#6697=AXIS2_PLACEMENT_3D('',#15967,#7551,#7552);
#6698=AXIS2_PLACEMENT_3D('',#15968,#7553,#7554);
#6699=AXIS2_PLACEMENT_3D('',#15971,#7555,#7556);
#6700=AXIS2_PLACEMENT_3D('',#15973,#7557,#7558);
#6701=AXIS2_PLACEMENT_3D('',#15974,#7559,#7560);
#6702=AXIS2_PLACEMENT_3D('',#15975,#7561,#7562);
#6703=AXIS2_PLACEMENT_3D('',#15978,#7563,#7564);
#6704=AXIS2_PLACEMENT_3D('',#15980,#7565,#7566);
#6705=AXIS2_PLACEMENT_3D('',#15981,#7567,#7568);
#6706=AXIS2_PLACEMENT_3D('',#15982,#7569,#7570);
#6707=AXIS2_PLACEMENT_3D('',#15985,#7571,#7572);
#6708=AXIS2_PLACEMENT_3D('',#15987,#7573,#7574);
#6709=AXIS2_PLACEMENT_3D('',#15988,#7575,#7576);
#6710=AXIS2_PLACEMENT_3D('',#15989,#7577,#7578);
#6711=AXIS2_PLACEMENT_3D('',#15992,#7579,#7580);
#6712=AXIS2_PLACEMENT_3D('',#15994,#7581,#7582);
#6713=AXIS2_PLACEMENT_3D('',#15995,#7583,#7584);
#6714=AXIS2_PLACEMENT_3D('',#15996,#7585,#7586);
#6715=AXIS2_PLACEMENT_3D('',#15999,#7587,#7588);
#6716=AXIS2_PLACEMENT_3D('',#16001,#7589,#7590);
#6717=AXIS2_PLACEMENT_3D('',#16002,#7591,#7592);
#6718=AXIS2_PLACEMENT_3D('',#16003,#7593,#7594);
#6719=AXIS2_PLACEMENT_3D('',#16006,#7595,#7596);
#6720=AXIS2_PLACEMENT_3D('',#16008,#7597,#7598);
#6721=AXIS2_PLACEMENT_3D('',#16009,#7599,#7600);
#6722=AXIS2_PLACEMENT_3D('',#16010,#7601,#7602);
#6723=AXIS2_PLACEMENT_3D('',#16013,#7603,#7604);
#6724=AXIS2_PLACEMENT_3D('',#16015,#7605,#7606);
#6725=AXIS2_PLACEMENT_3D('',#16016,#7607,#7608);
#6726=AXIS2_PLACEMENT_3D('',#16017,#7609,#7610);
#6727=AXIS2_PLACEMENT_3D('',#16020,#7613,#7614);
#6728=AXIS2_PLACEMENT_3D('',#16023,#7617,#7618);
#6729=AXIS2_PLACEMENT_3D('',#16026,#7621,#7622);
#6730=AXIS2_PLACEMENT_3D('',#16029,#7625,#7626);
#6731=AXIS2_PLACEMENT_3D('',#16032,#7629,#7630);
#6732=AXIS2_PLACEMENT_3D('',#16035,#7633,#7634);
#6733=AXIS2_PLACEMENT_3D('',#16038,#7637,#7638);
#6734=AXIS2_PLACEMENT_3D('',#16041,#7641,#7642);
#6735=AXIS2_PLACEMENT_3D('',#16044,#7645,#7646);
#6736=AXIS2_PLACEMENT_3D('',#16047,#7649,#7650);
#6737=AXIS2_PLACEMENT_3D('',#16050,#7653,#7654);
#6738=AXIS2_PLACEMENT_3D('',#16053,#7657,#7658);
#6739=AXIS2_PLACEMENT_3D('',#16054,#7659,#7660);
#6740=AXIS2_PLACEMENT_3D('',#16064,#7665,#7666);
#6741=AXIS2_PLACEMENT_3D('',#16066,#7667,#7668);
#6742=AXIS2_PLACEMENT_3D('',#16067,#7669,#7670);
#6743=AXIS2_PLACEMENT_3D('',#16068,#7671,#7672);
#6744=AXIS2_PLACEMENT_3D('',#16069,#7673,#7674);
#6745=AXIS2_PLACEMENT_3D('',#16079,#7679,#7680);
#6746=AXIS2_PLACEMENT_3D('',#16081,#7681,#7682);
#6747=AXIS2_PLACEMENT_3D('',#16082,#7683,#7684);
#6748=AXIS2_PLACEMENT_3D('',#16083,#7685,#7686);
#6749=AXIS2_PLACEMENT_3D('',#16085,#7688,#7689);
#6750=AXIS2_PLACEMENT_3D('',#16087,#7691,#7692);
#6751=AXIS2_PLACEMENT_3D('',#16090,#7695,#7696);
#6752=AXIS2_PLACEMENT_3D('',#16092,#7698,#7699);
#6753=AXIS2_PLACEMENT_3D('',#16094,#7701,#7702);
#6754=AXIS2_PLACEMENT_3D('',#16095,#7703,#7704);
#6755=AXIS2_PLACEMENT_3D('',#16096,#7705,#7706);
#6756=AXIS2_PLACEMENT_3D('',#16098,#7707,#7708);
#6757=AXIS2_PLACEMENT_3D('',#16101,#7710,#7711);
#6758=AXIS2_PLACEMENT_3D('',#16102,#7712,#7713);
#6759=AXIS2_PLACEMENT_3D('',#16104,#7714,#7715);
#6760=AXIS2_PLACEMENT_3D('',#16107,#7717,#7718);
#6761=AXIS2_PLACEMENT_3D('',#16108,#7719,#7720);
#6762=AXIS2_PLACEMENT_3D('',#16117,#7725,#7726);
#6763=AXIS2_PLACEMENT_3D('',#16123,#7730,#7731);
#6764=AXIS2_PLACEMENT_3D('',#16129,#7735,#7736);
#6765=AXIS2_PLACEMENT_3D('',#16132,#7739,#7740);
#6766=AXIS2_PLACEMENT_3D('',#16141,#7745,#7746);
#6767=AXIS2_PLACEMENT_3D('',#16147,#7750,#7751);
#6768=AXIS2_PLACEMENT_3D('',#16153,#7755,#7756);
#6769=AXIS2_PLACEMENT_3D('',#16156,#7759,#7760);
#6770=AXIS2_PLACEMENT_3D('',#16157,#7761,#7762);
#6771=AXIS2_PLACEMENT_3D('',#16158,#7763,#7764);
#6772=AXIS2_PLACEMENT_3D('',#16159,#7765,#7766);
#6773=AXIS2_PLACEMENT_3D('',#16161,#7767,#7768);
#6774=AXIS2_PLACEMENT_3D('',#16164,#7770,#7771);
#6775=AXIS2_PLACEMENT_3D('',#16165,#7772,#7773);
#6776=AXIS2_PLACEMENT_3D('',#16167,#7774,#7775);
#6777=AXIS2_PLACEMENT_3D('',#16170,#7777,#7778);
#6778=AXIS2_PLACEMENT_3D('',#16171,#7779,#7780);
#6779=AXIS2_PLACEMENT_3D('',#16173,#7781,#7782);
#6780=AXIS2_PLACEMENT_3D('',#16176,#7784,#7785);
#6781=AXIS2_PLACEMENT_3D('',#16177,#7786,#7787);
#6782=AXIS2_PLACEMENT_3D('',#16179,#7788,#7789);
#6783=AXIS2_PLACEMENT_3D('',#16182,#7791,#7792);
#6784=AXIS2_PLACEMENT_3D('',#16183,#7793,#7794);
#6785=AXIS2_PLACEMENT_3D('',#16192,#7799,#7800);
#6786=AXIS2_PLACEMENT_3D('',#16198,#7804,#7805);
#6787=AXIS2_PLACEMENT_3D('',#16204,#7809,#7810);
#6788=AXIS2_PLACEMENT_3D('',#16207,#7813,#7814);
#6789=AXIS2_PLACEMENT_3D('',#16216,#7819,#7820);
#6790=AXIS2_PLACEMENT_3D('',#16222,#7824,#7825);
#6791=AXIS2_PLACEMENT_3D('',#16228,#7829,#7830);
#6792=AXIS2_PLACEMENT_3D('',#16231,#7833,#7834);
#6793=AXIS2_PLACEMENT_3D('',#16240,#7839,#7840);
#6794=AXIS2_PLACEMENT_3D('',#16246,#7844,#7845);
#6795=AXIS2_PLACEMENT_3D('',#16252,#7849,#7850);
#6796=AXIS2_PLACEMENT_3D('',#16255,#7853,#7854);
#6797=AXIS2_PLACEMENT_3D('',#16264,#7859,#7860);
#6798=AXIS2_PLACEMENT_3D('',#16270,#7864,#7865);
#6799=AXIS2_PLACEMENT_3D('',#16276,#7869,#7870);
#6800=AXIS2_PLACEMENT_3D('',#16279,#7873,#7874);
#6801=AXIS2_PLACEMENT_3D('',#16280,#7875,#7876);
#6802=AXIS2_PLACEMENT_3D('',#16281,#7877,#7878);
#6803=AXIS2_PLACEMENT_3D('',#16282,#7879,#7880);
#6804=AXIS2_PLACEMENT_3D('',#16284,#7881,#7882);
#6805=AXIS2_PLACEMENT_3D('',#16287,#7884,#7885);
#6806=AXIS2_PLACEMENT_3D('',#16288,#7886,#7887);
#6807=AXIS2_PLACEMENT_3D('',#16297,#7892,#7893);
#6808=AXIS2_PLACEMENT_3D('',#16303,#7897,#7898);
#6809=AXIS2_PLACEMENT_3D('',#16309,#7902,#7903);
#6810=AXIS2_PLACEMENT_3D('',#16312,#7906,#7907);
#6811=AXIS2_PLACEMENT_3D('',#16313,#7908,#7909);
#6812=AXIS2_PLACEMENT_3D('',#16314,#7910,#7911);
#6813=AXIS2_PLACEMENT_3D('',#16315,#7912,#7913);
#6814=AXIS2_PLACEMENT_3D('',#16317,#7914,#7915);
#6815=AXIS2_PLACEMENT_3D('',#16320,#7917,#7918);
#6816=AXIS2_PLACEMENT_3D('',#16321,#7919,#7920);
#6817=AXIS2_PLACEMENT_3D('',#16330,#7925,#7926);
#6818=AXIS2_PLACEMENT_3D('',#16336,#7930,#7931);
#6819=AXIS2_PLACEMENT_3D('',#16342,#7935,#7936);
#6820=AXIS2_PLACEMENT_3D('',#16345,#7939,#7940);
#6821=AXIS2_PLACEMENT_3D('',#16346,#7941,#7942);
#6822=AXIS2_PLACEMENT_3D('',#16347,#7943,#7944);
#6823=AXIS2_PLACEMENT_3D('',#16348,#7945,#7946);
#6824=AXIS2_PLACEMENT_3D('',#16364,#7948,#7949);
#6825=AXIS2_PLACEMENT_3D('',#16372,#7950,#7951);
#6826=AXIS2_PLACEMENT_3D('',#16420,#7953,#7954);
#6827=AXIS2_PLACEMENT_3D('',#16468,#7956,#7957);
#6828=AXIS2_PLACEMENT_3D('',#16519,#7959,#7960);
#6829=AXIS2_PLACEMENT_3D('',#16570,#7962,#7963);
#6830=AXIS2_PLACEMENT_3D('',#16618,#7965,#7966);
#6831=AXIS2_PLACEMENT_3D('',#16666,#7968,#7969);
#6832=AXIS2_PLACEMENT_3D('',#16720,#7971,#7972);
#6833=AXIS2_PLACEMENT_3D('',#16768,#7974,#7975);
#6834=AXIS2_PLACEMENT_3D('',#16816,#7977,#7978);
#6835=AXIS2_PLACEMENT_3D('',#16832,#7980,#7981);
#6836=AXIS2_PLACEMENT_3D('',#16841,#7982,#7983);
#6837=AXIS2_PLACEMENT_3D('',#16866,#7985,#7986);
#6838=AXIS2_PLACEMENT_3D('',#16890,#7988,#7989);
#6839=AXIS2_PLACEMENT_3D('',#16915,#7991,#7992);
#6840=AXIS2_PLACEMENT_3D('',#16940,#7994,#7995);
#6841=AXIS2_PLACEMENT_3D('',#16964,#7997,#7998);
#6842=AXIS2_PLACEMENT_3D('',#16988,#8000,#8001);
#6843=AXIS2_PLACEMENT_3D('',#17014,#8003,#8004);
#6844=AXIS2_PLACEMENT_3D('',#17038,#8006,#8007);
#6845=AXIS2_PLACEMENT_3D('',#17062,#8009,#8010);
#6846=AXIS2_PLACEMENT_3D('',#17329,#8011,#8012);
#6847=AXIS2_PLACEMENT_3D('',#17360,#8014,#8015);
#6848=AXIS2_PLACEMENT_3D('',#17754,#8016,#8017);
#6849=AXIS2_PLACEMENT_3D('',#17765,#8018,#8019);
#6850=AXIS2_PLACEMENT_3D('',#18158,#8020,#8021);
#6851=AXIS2_PLACEMENT_3D('',#18159,#8022,#8023);
#6852=AXIS2_PLACEMENT_3D('',#18168,#8028,#8029);
#6853=AXIS2_PLACEMENT_3D('',#18174,#8033,#8034);
#6854=AXIS2_PLACEMENT_3D('',#18180,#8038,#8039);
#6855=AXIS2_PLACEMENT_3D('',#18186,#8043,#8044);
#6856=AXIS2_PLACEMENT_3D('',#18192,#8048,#8049);
#6857=AXIS2_PLACEMENT_3D('',#18195,#8052,#8053);
#6858=AXIS2_PLACEMENT_3D('',#18196,#8054,#8055);
#6859=AXIS2_PLACEMENT_3D('',#18198,#8056,#8057);
#6860=AXIS2_PLACEMENT_3D('',#18199,#8058,#8059);
#6861=AXIS2_PLACEMENT_3D('',#18202,#8061,#8062);
#6862=AXIS2_PLACEMENT_3D('',#18203,#8063,#8064);
#6863=AXIS2_PLACEMENT_3D('',#18204,#8065,#8066);
#6864=AXIS2_PLACEMENT_3D('',#18205,#8067,#8068);
#6865=AXIS2_PLACEMENT_3D('',#18206,#8069,#8070);
#6866=AXIS2_PLACEMENT_3D('',#18222,#8072,#8073);
#6867=AXIS2_PLACEMENT_3D('',#18230,#8074,#8075);
#6868=AXIS2_PLACEMENT_3D('',#18278,#8077,#8078);
#6869=AXIS2_PLACEMENT_3D('',#18326,#8080,#8081);
#6870=AXIS2_PLACEMENT_3D('',#18380,#8083,#8084);
#6871=AXIS2_PLACEMENT_3D('',#18428,#8086,#8087);
#6872=AXIS2_PLACEMENT_3D('',#18476,#8089,#8090);
#6873=AXIS2_PLACEMENT_3D('',#18530,#8092,#8093);
#6874=AXIS2_PLACEMENT_3D('',#18578,#8095,#8096);
#6875=AXIS2_PLACEMENT_3D('',#18626,#8098,#8099);
#6876=AXIS2_PLACEMENT_3D('',#18680,#8101,#8102);
#6877=AXIS2_PLACEMENT_3D('',#18728,#8104,#8105);
#6878=AXIS2_PLACEMENT_3D('',#18776,#8107,#8108);
#6879=AXIS2_PLACEMENT_3D('',#18830,#8110,#8111);
#6880=AXIS2_PLACEMENT_3D('',#18878,#8113,#8114);
#6881=AXIS2_PLACEMENT_3D('',#18926,#8116,#8117);
#6882=AXIS2_PLACEMENT_3D('',#18942,#8119,#8120);
#6883=AXIS2_PLACEMENT_3D('',#18951,#8121,#8122);
#6884=AXIS2_PLACEMENT_3D('',#18976,#8124,#8125);
#6885=AXIS2_PLACEMENT_3D('',#19000,#8127,#8128);
#6886=AXIS2_PLACEMENT_3D('',#19025,#8130,#8131);
#6887=AXIS2_PLACEMENT_3D('',#19050,#8133,#8134);
#6888=AXIS2_PLACEMENT_3D('',#19074,#8136,#8137);
#6889=AXIS2_PLACEMENT_3D('',#19099,#8139,#8140);
#6890=AXIS2_PLACEMENT_3D('',#19124,#8142,#8143);
#6891=AXIS2_PLACEMENT_3D('',#19148,#8145,#8146);
#6892=AXIS2_PLACEMENT_3D('',#19173,#8148,#8149);
#6893=AXIS2_PLACEMENT_3D('',#19198,#8151,#8152);
#6894=AXIS2_PLACEMENT_3D('',#19222,#8154,#8155);
#6895=AXIS2_PLACEMENT_3D('',#19247,#8157,#8158);
#6896=AXIS2_PLACEMENT_3D('',#19272,#8160,#8161);
#6897=AXIS2_PLACEMENT_3D('',#19296,#8163,#8164);
#6898=AXIS2_PLACEMENT_3D('',#19584,#8165,#8166);
#6899=AXIS2_PLACEMENT_3D('',#19618,#8168,#8169);
#6900=AXIS2_PLACEMENT_3D('',#20143,#8170,#8171);
#6901=AXIS2_PLACEMENT_3D('',#20154,#8172,#8173);
#6902=AXIS2_PLACEMENT_3D('',#20681,#8174,#8175);
#6903=AXIS2_PLACEMENT_3D('',#20682,#8176,#8177);
#6904=AXIS2_PLACEMENT_3D('',#20691,#8182,#8183);
#6905=AXIS2_PLACEMENT_3D('',#20697,#8187,#8188);
#6906=AXIS2_PLACEMENT_3D('',#20703,#8192,#8193);
#6907=AXIS2_PLACEMENT_3D('',#20709,#8197,#8198);
#6908=AXIS2_PLACEMENT_3D('',#20715,#8202,#8203);
#6909=AXIS2_PLACEMENT_3D('',#20718,#8206,#8207);
#6910=AXIS2_PLACEMENT_3D('',#20719,#8208,#8209);
#6911=AXIS2_PLACEMENT_3D('',#20721,#8210,#8211);
#6912=AXIS2_PLACEMENT_3D('',#20722,#8212,#8213);
#6913=AXIS2_PLACEMENT_3D('',#20725,#8215,#8216);
#6914=AXIS2_PLACEMENT_3D('',#20726,#8217,#8218);
#6915=AXIS2_PLACEMENT_3D('',#20727,#8219,#8220);
#6916=AXIS2_PLACEMENT_3D('',#20728,#8221,#8222);
#6917=AXIS2_PLACEMENT_3D('',#20729,#8223,#8224);
#6918=AXIS2_PLACEMENT_3D('',#20731,#8225,#8226);
#6919=AXIS2_PLACEMENT_3D('',#20734,#8228,#8229);
#6920=AXIS2_PLACEMENT_3D('',#20735,#8230,#8231);
#6921=AXIS2_PLACEMENT_3D('',#20737,#8232,#8233);
#6922=AXIS2_PLACEMENT_3D('',#20740,#8235,#8236);
#6923=AXIS2_PLACEMENT_3D('',#20741,#8237,#8238);
#6924=AXIS2_PLACEMENT_3D('',#20742,#8239,#8240);
#6925=AXIS2_PLACEMENT_3D('',#20743,#8241,#8242);
#6926=AXIS2_PLACEMENT_3D('',#20744,#8243,#8244);
#6927=AXIS2_PLACEMENT_3D('',#20754,#8246,#8247);
#6928=AXIS2_PLACEMENT_3D('',#20765,#8248,#8249);
#6929=AXIS2_PLACEMENT_3D('',#20816,#8251,#8252);
#6930=AXIS2_PLACEMENT_3D('',#20867,#8254,#8255);
#6931=AXIS2_PLACEMENT_3D('',#20915,#8257,#8258);
#6932=AXIS2_PLACEMENT_3D('',#20934,#8260,#8261);
#6933=AXIS2_PLACEMENT_3D('',#20954,#8262,#8263);
#6934=AXIS2_PLACEMENT_3D('',#20968,#8265,#8266);
#6935=AXIS2_PLACEMENT_3D('',#20978,#8267,#8268);
#6936=AXIS2_PLACEMENT_3D('',#21002,#8270,#8271);
#6937=AXIS2_PLACEMENT_3D('',#21027,#8273,#8274);
#6938=AXIS2_PLACEMENT_3D('',#21052,#8276,#8277);
#6939=AXIS2_PLACEMENT_3D('',#21063,#8279,#8280);
#6940=AXIS2_PLACEMENT_3D('',#21069,#8281,#8282);
#6941=AXIS2_PLACEMENT_3D('',#21801,#8283,#8284);
#6942=AXIS2_PLACEMENT_3D('',#21814,#8291,#8292);
#6943=AXIS2_PLACEMENT_3D('',#21815,#8293,#8294);
#6944=AXIS2_PLACEMENT_3D('',#21821,#8298,#8299);
#6945=AXIS2_PLACEMENT_3D('',#21825,#8302,#8303);
#6946=AXIS2_PLACEMENT_3D('',#21829,#8306,#8307);
#6947=AXIS2_PLACEMENT_3D('',#21833,#8310,#8311);
#6948=AXIS2_PLACEMENT_3D('',#21837,#8314,#8315);
#6949=AXIS2_PLACEMENT_3D('',#21839,#8317,#8318);
#6950=AXIS2_PLACEMENT_3D('',#21840,#8319,#8320);
#6951=AXIS2_PLACEMENT_3D('',#21841,#8321,#8322);
#6952=AXIS2_PLACEMENT_3D('',#21842,#8323,#8324);
#6953=AXIS2_PLACEMENT_3D('',#21843,#8325,#8326);
#6954=AXIS2_PLACEMENT_3D('',#21844,#8327,#8328);
#6955=AXIS2_PLACEMENT_3D('',#21845,#8329,#8330);
#6956=AXIS2_PLACEMENT_3D('',#21846,#8331,#8332);
#6957=AXIS2_PLACEMENT_3D('',#21847,#8333,#8334);
#6958=AXIS2_PLACEMENT_3D('',#21848,#8335,#8336);
#6959=AXIS2_PLACEMENT_3D('',#21849,#8337,#8338);
#6960=AXIS2_PLACEMENT_3D('',#21850,#8339,#8340);
#6961=AXIS2_PLACEMENT_3D('',#21851,#8341,#8342);
#6962=AXIS2_PLACEMENT_3D('',#21852,#8343,#8344);
#6963=AXIS2_PLACEMENT_3D('',#21853,#8345,#8346);
#6964=AXIS2_PLACEMENT_3D('',#21854,#8347,#8348);
#6965=AXIS2_PLACEMENT_3D('',#21855,#8349,#8350);
#6966=AXIS2_PLACEMENT_3D('',#21856,#8351,#8352);
#6967=DIRECTION('axis',(0.,0.,1.));
#6968=DIRECTION('refdir',(1.,0.,0.));
#6969=DIRECTION('axis',(0.,0.,1.));
#6970=DIRECTION('refdir',(1.,0.,0.));
#6971=DIRECTION('center_axis',(0.,0.,-1.));
#6972=DIRECTION('ref_axis',(1.,0.,0.));
#6973=DIRECTION('',(0.,0.,-1.));
#6974=DIRECTION('center_axis',(0.,0.,-1.));
#6975=DIRECTION('ref_axis',(1.,0.,0.));
#6976=DIRECTION('center_axis',(0.,0.,-1.));
#6977=DIRECTION('ref_axis',(1.,0.,0.));
#6978=DIRECTION('',(0.,0.,-1.));
#6979=DIRECTION('center_axis',(0.,0.,-1.));
#6980=DIRECTION('ref_axis',(1.,0.,0.));
#6981=DIRECTION('',(0.,0.,-1.));
#6982=DIRECTION('center_axis',(0.,0.,-1.));
#6983=DIRECTION('ref_axis',(1.,0.,0.));
#6984=DIRECTION('',(0.,0.,-1.));
#6985=DIRECTION('center_axis',(0.,0.,-1.));
#6986=DIRECTION('ref_axis',(1.,0.,0.));
#6987=DIRECTION('',(0.,0.,-1.));
#6988=DIRECTION('center_axis',(0.,0.,-1.));
#6989=DIRECTION('ref_axis',(1.,0.,0.));
#6990=DIRECTION('',(0.,0.,-1.));
#6991=DIRECTION('center_axis',(0.,0.,-1.));
#6992=DIRECTION('ref_axis',(1.,0.,0.));
#6993=DIRECTION('',(0.,0.,-1.));
#6994=DIRECTION('center_axis',(0.,0.,-1.));
#6995=DIRECTION('ref_axis',(1.,0.,0.));
#6996=DIRECTION('',(0.,0.,-1.));
#6997=DIRECTION('center_axis',(0.,0.,-1.));
#6998=DIRECTION('ref_axis',(1.,0.,0.));
#6999=DIRECTION('',(0.,0.,-1.));
#7000=DIRECTION('center_axis',(0.,0.,-1.));
#7001=DIRECTION('ref_axis',(1.,0.,0.));
#7002=DIRECTION('',(0.,0.,-1.));
#7003=DIRECTION('center_axis',(0.,0.,-1.));
#7004=DIRECTION('ref_axis',(0.938435415243825,-0.345454731355861,0.));
#7005=DIRECTION('',(0.,0.,-1.));
#7006=DIRECTION('center_axis',(0.,0.,-1.));
#7007=DIRECTION('ref_axis',(1.,0.,0.));
#7008=DIRECTION('center_axis',(0.,0.,-1.));
#7009=DIRECTION('ref_axis',(1.,0.,0.));
#7010=DIRECTION('',(0.,0.,-1.));
#7011=DIRECTION('center_axis',(0.,0.,-1.));
#7012=DIRECTION('ref_axis',(1.,0.,0.));
#7013=DIRECTION('center_axis',(0.,0.,-1.));
#7014=DIRECTION('ref_axis',(1.,0.,0.));
#7015=DIRECTION('',(0.,0.,-1.));
#7016=DIRECTION('center_axis',(0.,0.,-1.));
#7017=DIRECTION('ref_axis',(1.,0.,0.));
#7018=DIRECTION('',(0.,0.,-1.));
#7019=DIRECTION('center_axis',(0.,0.,-1.));
#7020=DIRECTION('ref_axis',(1.,0.,0.));
#7021=DIRECTION('',(0.,0.,-1.));
#7022=DIRECTION('center_axis',(0.,0.,-1.));
#7023=DIRECTION('ref_axis',(1.,0.,0.));
#7024=DIRECTION('',(0.,0.,-1.));
#7025=DIRECTION('center_axis',(0.,0.,-1.));
#7026=DIRECTION('ref_axis',(1.,0.,0.));
#7027=DIRECTION('',(0.,0.,-1.));
#7028=DIRECTION('center_axis',(0.,0.,-1.));
#7029=DIRECTION('ref_axis',(1.,0.,0.));
#7030=DIRECTION('',(0.,0.,-1.));
#7031=DIRECTION('center_axis',(0.,0.,-1.));
#7032=DIRECTION('ref_axis',(1.,0.,0.));
#7033=DIRECTION('',(0.,0.,-1.));
#7034=DIRECTION('center_axis',(0.,0.,-1.));
#7035=DIRECTION('ref_axis',(1.,0.,0.));
#7036=DIRECTION('',(0.,0.,-1.));
#7037=DIRECTION('center_axis',(0.,0.,-1.));
#7038=DIRECTION('ref_axis',(1.,0.,0.));
#7039=DIRECTION('',(0.,0.,-1.));
#7040=DIRECTION('center_axis',(0.,0.,-1.));
#7041=DIRECTION('ref_axis',(0.938435444148243,-0.34545465283636,0.));
#7042=DIRECTION('',(0.,0.,-1.));
#7043=DIRECTION('center_axis',(0.,0.,-1.));
#7044=DIRECTION('ref_axis',(1.,0.,0.));
#7045=DIRECTION('center_axis',(0.,0.,-1.));
#7046=DIRECTION('ref_axis',(1.,0.,0.));
#7047=DIRECTION('',(0.,0.,-1.));
#7048=DIRECTION('center_axis',(0.,0.,-1.));
#7049=DIRECTION('ref_axis',(1.,0.,0.));
#7050=DIRECTION('center_axis',(0.,0.,-1.));
#7051=DIRECTION('ref_axis',(1.,0.,0.));
#7052=DIRECTION('',(0.,0.,-1.));
#7053=DIRECTION('center_axis',(0.,0.,-1.));
#7054=DIRECTION('ref_axis',(1.,0.,0.));
#7055=DIRECTION('',(0.,0.,-1.));
#7056=DIRECTION('center_axis',(0.,0.,-1.));
#7057=DIRECTION('ref_axis',(1.,0.,0.));
#7058=DIRECTION('',(0.,0.,-1.));
#7059=DIRECTION('center_axis',(0.,0.,-1.));
#7060=DIRECTION('ref_axis',(1.,0.,0.));
#7061=DIRECTION('',(0.,0.,-1.));
#7062=DIRECTION('center_axis',(0.,0.,-1.));
#7063=DIRECTION('ref_axis',(1.,0.,0.));
#7064=DIRECTION('',(0.,0.,-1.));
#7065=DIRECTION('center_axis',(0.,0.,-1.));
#7066=DIRECTION('ref_axis',(1.,0.,0.));
#7067=DIRECTION('',(0.,0.,-1.));
#7068=DIRECTION('center_axis',(0.,0.,-1.));
#7069=DIRECTION('ref_axis',(1.,0.,0.));
#7070=DIRECTION('',(0.,0.,-1.));
#7071=DIRECTION('center_axis',(0.,0.,-1.));
#7072=DIRECTION('ref_axis',(1.,0.,0.));
#7073=DIRECTION('',(0.,0.,-1.));
#7074=DIRECTION('center_axis',(0.,0.,-1.));
#7075=DIRECTION('ref_axis',(1.,0.,0.));
#7076=DIRECTION('',(0.,0.,-1.));
#7077=DIRECTION('center_axis',(0.,0.,-1.));
#7078=DIRECTION('ref_axis',(0.938435456291759,-0.345454619848221,0.));
#7079=DIRECTION('',(0.,0.,-1.));
#7080=DIRECTION('center_axis',(0.,0.,-1.));
#7081=DIRECTION('ref_axis',(1.,0.,0.));
#7082=DIRECTION('center_axis',(0.,0.,-1.));
#7083=DIRECTION('ref_axis',(1.,0.,0.));
#7084=DIRECTION('center_axis',(0.,0.,-1.));
#7085=DIRECTION('ref_axis',(1.,0.,0.));
#7086=DIRECTION('',(0.,0.,-1.));
#7087=DIRECTION('center_axis',(0.,0.,-1.));
#7088=DIRECTION('ref_axis',(1.,0.,0.));
#7089=DIRECTION('center_axis',(0.,0.,-1.));
#7090=DIRECTION('ref_axis',(1.,0.,0.));
#7091=DIRECTION('',(0.,0.,-1.));
#7092=DIRECTION('center_axis',(0.,0.,-1.));
#7093=DIRECTION('ref_axis',(1.,0.,0.));
#7094=DIRECTION('',(0.,0.,-1.));
#7095=DIRECTION('center_axis',(0.,0.,-1.));
#7096=DIRECTION('ref_axis',(1.,0.,0.));
#7097=DIRECTION('',(0.,0.,-1.));
#7098=DIRECTION('center_axis',(0.,0.,-1.));
#7099=DIRECTION('ref_axis',(1.,0.,0.));
#7100=DIRECTION('',(0.,0.,-1.));
#7101=DIRECTION('center_axis',(0.,0.,-1.));
#7102=DIRECTION('ref_axis',(1.,0.,0.));
#7103=DIRECTION('',(0.,0.,-1.));
#7104=DIRECTION('center_axis',(0.,0.,-1.));
#7105=DIRECTION('ref_axis',(1.,0.,0.));
#7106=DIRECTION('',(0.,0.,-1.));
#7107=DIRECTION('center_axis',(0.,0.,-1.));
#7108=DIRECTION('ref_axis',(1.,0.,0.));
#7109=DIRECTION('',(0.,0.,-1.));
#7110=DIRECTION('center_axis',(0.,0.,-1.));
#7111=DIRECTION('ref_axis',(1.,0.,0.));
#7112=DIRECTION('',(0.,0.,-1.));
#7113=DIRECTION('center_axis',(0.,0.,-1.));
#7114=DIRECTION('ref_axis',(1.,0.,0.));
#7115=DIRECTION('',(0.,0.,-1.));
#7116=DIRECTION('center_axis',(0.,0.,-1.));
#7117=DIRECTION('ref_axis',(0.938435399436813,-0.345454774295956,0.));
#7118=DIRECTION('',(0.,0.,-1.));
#7119=DIRECTION('center_axis',(0.,0.,-1.));
#7120=DIRECTION('ref_axis',(1.,0.,0.));
#7121=DIRECTION('center_axis',(0.,0.,-1.));
#7122=DIRECTION('ref_axis',(1.,0.,0.));
#7123=DIRECTION('center_axis',(0.,0.,-1.));
#7124=DIRECTION('ref_axis',(-0.770520550489697,0.637415156136921,0.));
#7125=DIRECTION('',(1.22464679914735E-16,-5.30860927203279E-30,-1.));
#7126=DIRECTION('center_axis',(0.,0.,1.));
#7127=DIRECTION('ref_axis',(1.,-4.32256196471651E-14,0.));
#7128=DIRECTION('center_axis',(0.,0.,-1.));
#7129=DIRECTION('ref_axis',(1.,-4.32256196471651E-14,0.));
#7130=DIRECTION('',(1.22464679914735E-16,-5.30860927203279E-30,-1.));
#7131=DIRECTION('center_axis',(0.,0.,-1.));
#7132=DIRECTION('ref_axis',(1.,-4.32256196471651E-14,0.));
#7133=DIRECTION('',(1.22464679914735E-16,-5.30860927203279E-30,-1.));
#7134=DIRECTION('center_axis',(0.,0.,-1.));
#7135=DIRECTION('ref_axis',(1.,-4.32256196471651E-14,0.));
#7136=DIRECTION('',(1.22464679914735E-16,-5.30860927203279E-30,-1.));
#7137=DIRECTION('center_axis',(0.,0.,-1.));
#7138=DIRECTION('ref_axis',(1.,-4.32256196471651E-14,0.));
#7139=DIRECTION('',(1.22464679914735E-16,-5.30860927203279E-30,-1.));
#7140=DIRECTION('center_axis',(0.,0.,-1.));
#7141=DIRECTION('ref_axis',(1.,-4.32256196471651E-14,0.));
#7142=DIRECTION('',(1.22464679914735E-16,-5.30860927203279E-30,-1.));
#7143=DIRECTION('center_axis',(0.,0.,-1.));
#7144=DIRECTION('ref_axis',(1.,-4.32256196471651E-14,0.));
#7145=DIRECTION('',(1.22464679914735E-16,-5.30860927203279E-30,-1.));
#7146=DIRECTION('center_axis',(0.,0.,-1.));
#7147=DIRECTION('ref_axis',(1.,-4.32256196471651E-14,0.));
#7148=DIRECTION('',(1.22464679914735E-16,-5.30860927203279E-30,-1.));
#7149=DIRECTION('center_axis',(0.,0.,-1.));
#7150=DIRECTION('ref_axis',(1.,-4.32256196471651E-14,0.));
#7151=DIRECTION('',(1.22464679914735E-16,-5.30860927203279E-30,-1.));
#7152=DIRECTION('center_axis',(0.,0.,-1.));
#7153=DIRECTION('ref_axis',(1.,-4.32256196471651E-14,0.));
#7154=DIRECTION('',(1.22464679914735E-16,-5.30860927203279E-30,-1.));
#7155=DIRECTION('center_axis',(0.,0.,-1.));
#7156=DIRECTION('ref_axis',(1.,-4.32256196471651E-14,0.));
#7157=DIRECTION('',(1.22464679914735E-16,-5.30860927203279E-30,-1.));
#7158=DIRECTION('center_axis',(0.,0.,-1.));
#7159=DIRECTION('ref_axis',(-0.60934875646219,-0.792902322482399,0.));
#7160=DIRECTION('',(1.22464679914735E-16,-5.30860927203279E-30,-1.));
#7161=DIRECTION('center_axis',(0.,0.,-1.));
#7162=DIRECTION('ref_axis',(1.,-4.32256196471651E-14,0.));
#7163=DIRECTION('center_axis',(0.,0.,-1.));
#7164=DIRECTION('ref_axis',(-0.770520310070594,0.637415446760365,0.));
#7165=DIRECTION('',(1.22464679914735E-16,-5.17626898017763E-30,-1.));
#7166=DIRECTION('center_axis',(0.,0.,1.));
#7167=DIRECTION('ref_axis',(1.,-4.2144979155986E-14,0.));
#7168=DIRECTION('center_axis',(0.,0.,-1.));
#7169=DIRECTION('ref_axis',(1.,-4.2144979155986E-14,0.));
#7170=DIRECTION('',(1.22464679914735E-16,-5.17626898017763E-30,-1.));
#7171=DIRECTION('center_axis',(0.,0.,-1.));
#7172=DIRECTION('ref_axis',(1.,-4.2144979155986E-14,0.));
#7173=DIRECTION('',(1.22464679914735E-16,-5.17626898017763E-30,-1.));
#7174=DIRECTION('center_axis',(0.,0.,-1.));
#7175=DIRECTION('ref_axis',(1.,-4.2144979155986E-14,0.));
#7176=DIRECTION('',(1.22464679914735E-16,-5.17626898017763E-30,-1.));
#7177=DIRECTION('center_axis',(0.,0.,-1.));
#7178=DIRECTION('ref_axis',(1.,-4.2144979155986E-14,0.));
#7179=DIRECTION('',(1.22464679914735E-16,-5.17626898017763E-30,-1.));
#7180=DIRECTION('center_axis',(0.,0.,-1.));
#7181=DIRECTION('ref_axis',(1.,-4.2144979155986E-14,0.));
#7182=DIRECTION('',(1.22464679914735E-16,-5.17626898017763E-30,-1.));
#7183=DIRECTION('center_axis',(0.,0.,-1.));
#7184=DIRECTION('ref_axis',(1.,-4.2144979155986E-14,0.));
#7185=DIRECTION('',(1.22464679914735E-16,-5.17626898017763E-30,-1.));
#7186=DIRECTION('center_axis',(0.,0.,-1.));
#7187=DIRECTION('ref_axis',(1.,-4.2144979155986E-14,0.));
#7188=DIRECTION('',(1.22464679914735E-16,-5.17626898017763E-30,-1.));
#7189=DIRECTION('center_axis',(0.,0.,-1.));
#7190=DIRECTION('ref_axis',(1.,-4.2144979155986E-14,0.));
#7191=DIRECTION('',(1.22464679914735E-16,-5.17626898017763E-30,-1.));
#7192=DIRECTION('center_axis',(0.,0.,-1.));
#7193=DIRECTION('ref_axis',(1.,-4.2144979155986E-14,0.));
#7194=DIRECTION('',(1.22464679914735E-16,-5.17626898017763E-30,-1.));
#7195=DIRECTION('center_axis',(0.,0.,-1.));
#7196=DIRECTION('ref_axis',(1.,-4.2144979155986E-14,0.));
#7197=DIRECTION('',(1.22464679914735E-16,-5.17626898017763E-30,-1.));
#7198=DIRECTION('center_axis',(0.,0.,-1.));
#7199=DIRECTION('ref_axis',(-0.609348813471299,-0.792902278670657,0.));
#7200=DIRECTION('',(1.22464679914735E-16,-5.17626898017763E-30,-1.));
#7201=DIRECTION('center_axis',(0.,0.,-1.));
#7202=DIRECTION('ref_axis',(1.,-4.2144979155986E-14,0.));
#7203=DIRECTION('center_axis',(0.,0.,-1.));
#7204=DIRECTION('ref_axis',(-0.770520589723051,0.637415108710832,0.));
#7205=DIRECTION('',(1.22464679914735E-16,-5.37477941796036E-30,-1.));
#7206=DIRECTION('center_axis',(0.,0.,1.));
#7207=DIRECTION('ref_axis',(1.,-4.37659398927547E-14,0.));
#7208=DIRECTION('center_axis',(0.,0.,-1.));
#7209=DIRECTION('ref_axis',(1.,-4.37659398927547E-14,0.));
#7210=DIRECTION('',(1.22464679914735E-16,-5.37477941796036E-30,-1.));
#7211=DIRECTION('center_axis',(0.,0.,-1.));
#7212=DIRECTION('ref_axis',(1.,-4.37659398927547E-14,0.));
#7213=DIRECTION('',(1.22464679914735E-16,-5.37477941796036E-30,-1.));
#7214=DIRECTION('center_axis',(0.,0.,-1.));
#7215=DIRECTION('ref_axis',(1.,-4.37659398927547E-14,0.));
#7216=DIRECTION('',(1.22464679914735E-16,-5.37477941796036E-30,-1.));
#7217=DIRECTION('center_axis',(0.,0.,-1.));
#7218=DIRECTION('ref_axis',(1.,-4.37659398927547E-14,0.));
#7219=DIRECTION('',(1.22464679914735E-16,-5.37477941796036E-30,-1.));
#7220=DIRECTION('center_axis',(0.,0.,-1.));
#7221=DIRECTION('ref_axis',(1.,-4.37659398927547E-14,0.));
#7222=DIRECTION('',(1.22464679914735E-16,-5.37477941796036E-30,-1.));
#7223=DIRECTION('center_axis',(0.,0.,-1.));
#7224=DIRECTION('ref_axis',(1.,-4.37659398927547E-14,0.));
#7225=DIRECTION('',(1.22464679914735E-16,-5.37477941796036E-30,-1.));
#7226=DIRECTION('center_axis',(0.,0.,-1.));
#7227=DIRECTION('ref_axis',(1.,-4.37659398927547E-14,0.));
#7228=DIRECTION('',(1.22464679914735E-16,-5.37477941796036E-30,-1.));
#7229=DIRECTION('center_axis',(0.,0.,-1.));
#7230=DIRECTION('ref_axis',(1.,-4.37659398927547E-14,0.));
#7231=DIRECTION('',(1.22464679914735E-16,-5.37477941796036E-30,-1.));
#7232=DIRECTION('center_axis',(0.,0.,-1.));
#7233=DIRECTION('ref_axis',(1.,-4.37659398927547E-14,0.));
#7234=DIRECTION('',(1.22464679914735E-16,-5.37477941796036E-30,-1.));
#7235=DIRECTION('center_axis',(0.,0.,-1.));
#7236=DIRECTION('ref_axis',(1.,-4.37659398927547E-14,0.));
#7237=DIRECTION('',(1.22464679914735E-16,-5.37477941796036E-30,-1.));
#7238=DIRECTION('center_axis',(0.,0.,-1.));
#7239=DIRECTION('ref_axis',(-0.609348731823397,-0.792902341417414,0.));
#7240=DIRECTION('',(1.22464679914735E-16,-5.37477941796036E-30,-1.));
#7241=DIRECTION('center_axis',(0.,0.,-1.));
#7242=DIRECTION('ref_axis',(1.,-4.37659398927547E-14,0.));
#7243=DIRECTION('center_axis',(0.,0.,-1.));
#7244=DIRECTION('ref_axis',(-0.770520370143733,0.637415374142769,0.));
#7245=DIRECTION('',(1.22464679914735E-16,-5.30860927203279E-30,-1.));
#7246=DIRECTION('center_axis',(0.,0.,1.));
#7247=DIRECTION('ref_axis',(1.,-4.32256196471651E-14,0.));
#7248=DIRECTION('center_axis',(0.,0.,-1.));
#7249=DIRECTION('ref_axis',(1.,-4.32256196471651E-14,0.));
#7250=DIRECTION('',(1.22464679914735E-16,-5.30860927203279E-30,-1.));
#7251=DIRECTION('center_axis',(0.,0.,-1.));
#7252=DIRECTION('ref_axis',(1.,-4.32256196471651E-14,0.));
#7253=DIRECTION('',(1.22464679914735E-16,-5.30860927203279E-30,-1.));
#7254=DIRECTION('center_axis',(0.,0.,-1.));
#7255=DIRECTION('ref_axis',(1.,-4.32256196471651E-14,0.));
#7256=DIRECTION('',(1.22464679914735E-16,-5.30860927203279E-30,-1.));
#7257=DIRECTION('center_axis',(0.,0.,-1.));
#7258=DIRECTION('ref_axis',(1.,-4.32256196471651E-14,0.));
#7259=DIRECTION('',(1.22464679914735E-16,-5.30860927203279E-30,-1.));
#7260=DIRECTION('center_axis',(0.,0.,-1.));
#7261=DIRECTION('ref_axis',(1.,-4.32256196471651E-14,0.));
#7262=DIRECTION('',(1.22464679914735E-16,-5.30860927203279E-30,-1.));
#7263=DIRECTION('center_axis',(0.,0.,-1.));
#7264=DIRECTION('ref_axis',(1.,-4.32256196471651E-14,0.));
#7265=DIRECTION('',(1.22464679914735E-16,-5.30860927203279E-30,-1.));
#7266=DIRECTION('center_axis',(0.,0.,-1.));
#7267=DIRECTION('ref_axis',(1.,-4.32256196471651E-14,0.));
#7268=DIRECTION('',(1.22464679914735E-16,-5.30860927203279E-30,-1.));
#7269=DIRECTION('center_axis',(0.,0.,-1.));
#7270=DIRECTION('ref_axis',(1.,-4.32256196471651E-14,0.));
#7271=DIRECTION('',(1.22464679914735E-16,-5.30860927203279E-30,-1.));
#7272=DIRECTION('center_axis',(0.,0.,-1.));
#7273=DIRECTION('ref_axis',(1.,-4.32256196471651E-14,0.));
#7274=DIRECTION('',(1.22464679914735E-16,-5.30860927203279E-30,-1.));
#7275=DIRECTION('center_axis',(0.,0.,-1.));
#7276=DIRECTION('ref_axis',(1.,-4.32256196471651E-14,0.));
#7277=DIRECTION('',(1.22464679914735E-16,-5.30860927203279E-30,-1.));
#7278=DIRECTION('center_axis',(0.,0.,-1.));
#7279=DIRECTION('ref_axis',(-0.6093487836746,-0.792902301569547,0.));
#7280=DIRECTION('',(1.22464679914735E-16,-5.30860927203279E-30,-1.));
#7281=DIRECTION('center_axis',(0.,0.,-1.));
#7282=DIRECTION('ref_axis',(1.,-4.32256196471651E-14,0.));
#7283=DIRECTION('center_axis',(0.707106781186548,-0.707106781186547,0.));
#7284=DIRECTION('ref_axis',(-0.5,-0.499999999999999,0.707106781186548));
#7285=DIRECTION('',(-0.707106781186548,0.707106781186547,0.));
#7286=DIRECTION('center_axis',(0.923879532511287,-0.38268343236509,0.));
#7287=DIRECTION('ref_axis',(0.38268343236509,0.923879532511287,0.));
#7288=DIRECTION('',(0.707106781186548,-0.707106781186547,0.));
#7289=DIRECTION('center_axis',(0.38268343236509,-0.923879532511287,-9.37720122241284E-16));
#7290=DIRECTION('ref_axis',(0.923879532511287,0.38268343236509,-2.26385663682506E-15));
#7291=DIRECTION('center_axis',(1.,0.,0.));
#7292=DIRECTION('ref_axis',(0.,-0.707106781186547,0.707106781186548));
#7293=DIRECTION('',(-1.,0.,0.));
#7294=DIRECTION('center_axis',(0.923879532511287,0.38268343236509,0.));
#7295=DIRECTION('ref_axis',(-0.38268343236509,0.923879532511287,0.));
#7296=DIRECTION('',(1.,0.,0.));
#7297=DIRECTION('center_axis',(0.707106781186548,0.707106781186547,0.));
#7298=DIRECTION('ref_axis',(0.499999999999999,-0.5,0.707106781186548));
#7299=DIRECTION('',(-0.707106781186548,-0.707106781186547,0.));
#7300=DIRECTION('center_axis',(0.38268343236509,0.923879532511287,0.));
#7301=DIRECTION('ref_axis',(-0.923879532511287,0.38268343236509,0.));
#7302=DIRECTION('',(0.707106781186548,0.707106781186547,0.));
#7303=DIRECTION('center_axis',(0.,1.,0.));
#7304=DIRECTION('ref_axis',(0.707106781186547,0.,0.707106781186548));
#7305=DIRECTION('',(0.,-1.,0.));
#7306=DIRECTION('center_axis',(-0.707106781186548,0.707106781186548,0.));
#7307=DIRECTION('ref_axis',(-0.707106781186547,-0.707106781186547,0.));
#7308=DIRECTION('',(0.,1.,0.));
#7309=DIRECTION('center_axis',(-1.,0.,0.));
#7310=DIRECTION('ref_axis',(0.,0.707106781186547,0.707106781186548));
#7311=DIRECTION('',(-1.,0.,0.));
#7312=DIRECTION('',(1.,0.,0.));
#7313=DIRECTION('center_axis',(-0.707106781186548,-0.707106781186548,0.));
#7314=DIRECTION('ref_axis',(0.707106781186547,-0.707106781186547,0.));
#7315=DIRECTION('center_axis',(0.,-1.,0.));
#7316=DIRECTION('ref_axis',(-0.707106781186547,0.,0.707106781186548));
#7317=DIRECTION('',(0.,-1.,0.));
#7318=DIRECTION('',(0.,1.,0.));
#7319=DIRECTION('center_axis',(0.,1.,0.));
#7320=DIRECTION('ref_axis',(-1.,0.,0.));
#7321=DIRECTION('',(0.,0.,1.));
#7322=DIRECTION('',(1.,0.,0.));
#7323=DIRECTION('',(1.,0.,0.));
#7324=DIRECTION('',(1.,0.,0.));
#7325=DIRECTION('',(0.,0.,1.));
#7326=DIRECTION('center_axis',(-1.,0.,0.));
#7327=DIRECTION('ref_axis',(0.,-1.,0.));
#7328=DIRECTION('',(0.,0.,1.));
#7329=DIRECTION('',(0.,1.,0.));
#7330=DIRECTION('',(0.,1.,0.));
#7331=DIRECTION('center_axis',(-0.707106781186547,-0.707106781186548,0.));
#7332=DIRECTION('ref_axis',(0.707106781186548,-0.707106781186547,0.));
#7333=DIRECTION('',(0.,0.,1.));
#7334=DIRECTION('',(-0.707106781186548,0.707106781186547,0.));
#7335=DIRECTION('center_axis',(0.,0.,1.));
#7336=DIRECTION('ref_axis',(1.,0.,0.));
#7337=DIRECTION('',(0.,-1.,0.));
#7338=DIRECTION('center_axis',(0.,0.,1.));
#7339=DIRECTION('ref_axis',(-1.,-1.22464679914735E-16,0.));
#7340=DIRECTION('',(0.,-1.,0.));
#7341=DIRECTION('',(1.,0.,0.));
#7342=DIRECTION('',(0.,1.,0.));
#7343=DIRECTION('center_axis',(0.,0.,1.));
#7344=DIRECTION('ref_axis',(-1.,-1.22464679914735E-16,0.));
#7345=DIRECTION('center_axis',(0.,0.,1.));
#7346=DIRECTION('ref_axis',(-1.,-1.22464679914735E-16,0.));
#7347=DIRECTION('',(0.,1.,0.));
#7348=DIRECTION('',(-1.,0.,0.));
#7349=DIRECTION('center_axis',(0.,1.,0.));
#7350=DIRECTION('ref_axis',(0.707106781186546,0.,0.707106781186549));
#7351=DIRECTION('center_axis',(0.707106781186547,0.707106781186548,1.57009245868377E-15));
#7352=DIRECTION('ref_axis',(0.707106781186548,-0.707106781186547,1.57009245868377E-15));
#7353=DIRECTION('',(0.,1.,0.));
#7354=DIRECTION('center_axis',(-0.707106781186547,0.707106781186548,7.85046229341886E-16));
#7355=DIRECTION('ref_axis',(0.707106781186548,0.707106781186547,7.85046229341885E-16));
#7356=DIRECTION('center_axis',(1.,0.,0.));
#7357=DIRECTION('ref_axis',(0.,-0.707106781186545,0.70710678118655));
#7358=DIRECTION('center_axis',(0.707106781186547,-0.707106781186548,7.85046229341886E-16));
#7359=DIRECTION('ref_axis',(-0.707106781186548,-0.707106781186547,7.85046229341885E-16));
#7360=DIRECTION('',(1.,0.,0.));
#7361=DIRECTION('center_axis',(0.,-1.,0.));
#7362=DIRECTION('ref_axis',(-0.707106781186546,0.,0.707106781186549));
#7363=DIRECTION('center_axis',(-0.707106781186547,-0.707106781186548,1.57009245868377E-15));
#7364=DIRECTION('ref_axis',(-0.707106781186548,0.707106781186547,1.57009245868377E-15));
#7365=DIRECTION('',(0.,-1.,0.));
#7366=DIRECTION('center_axis',(-1.,0.,0.));
#7367=DIRECTION('ref_axis',(0.,0.707106781186545,0.70710678118655));
#7368=DIRECTION('',(-1.,0.,0.));
#7369=DIRECTION('center_axis',(0.,1.,0.));
#7370=DIRECTION('ref_axis',(-1.,0.,0.));
#7371=DIRECTION('',(0.,0.,1.));
#7372=DIRECTION('',(-1.,0.,0.));
#7373=DIRECTION('',(0.,0.,1.));
#7374=DIRECTION('center_axis',(1.,0.,0.));
#7375=DIRECTION('ref_axis',(0.,1.,0.));
#7376=DIRECTION('',(0.,0.,1.));
#7377=DIRECTION('',(0.,1.,0.));
#7378=DIRECTION('center_axis',(0.,0.,-1.));
#7379=DIRECTION('ref_axis',(-1.,0.,0.));
#7380=DIRECTION('center_axis',(-1.22464679914735E-16,-1.,0.));
#7381=DIRECTION('ref_axis',(1.,-1.22464679914735E-16,0.));
#7382=DIRECTION('center_axis',(0.,0.,-1.));
#7383=DIRECTION('ref_axis',(-1.,-1.22464679914735E-16,0.));
#7384=DIRECTION('center_axis',(0.,0.,-1.));
#7385=DIRECTION('ref_axis',(-1.,-1.22464679914735E-16,0.));
#7386=DIRECTION('center_axis',(0.,0.,-1.));
#7387=DIRECTION('ref_axis',(-1.,0.,0.));
#7388=DIRECTION('center_axis',(-1.22464679914735E-16,-1.,0.));
#7389=DIRECTION('ref_axis',(1.,-1.22464679914735E-16,0.));
#7390=DIRECTION('center_axis',(0.,0.,-1.));
#7391=DIRECTION('ref_axis',(-1.,-1.22464679914735E-16,0.));
#7392=DIRECTION('center_axis',(0.,0.,-1.));
#7393=DIRECTION('ref_axis',(-1.,-1.22464679914735E-16,0.));
#7394=DIRECTION('center_axis',(0.,0.,-1.));
#7395=DIRECTION('ref_axis',(1.,0.,0.));
#7396=DIRECTION('',(0.,0.,-1.));
#7397=DIRECTION('center_axis',(0.,0.,1.));
#7398=DIRECTION('ref_axis',(1.,0.,0.));
#7399=DIRECTION('center_axis',(0.,0.,-1.));
#7400=DIRECTION('ref_axis',(1.,0.,0.));
#7401=DIRECTION('',(0.,0.,-1.));
#7402=DIRECTION('center_axis',(0.,0.,1.));
#7403=DIRECTION('ref_axis',(1.,0.,0.));
#7404=DIRECTION('center_axis',(0.,0.,-1.));
#7405=DIRECTION('ref_axis',(1.,-4.32256196471651E-14,0.));
#7406=DIRECTION('center_axis',(0.,0.,1.));
#7407=DIRECTION('ref_axis',(1.,0.,0.));
#7408=DIRECTION('',(0.,-1.,0.));
#7409=DIRECTION('',(-0.707106781186547,-0.707106781186547,0.));
#7410=DIRECTION('',(-1.,0.,0.));
#7411=DIRECTION('',(-0.707106781186547,0.707106781186547,0.));
#7412=DIRECTION('',(0.,1.,0.));
#7413=DIRECTION('',(1.,0.,0.));
#7414=DIRECTION('',(1.,0.,0.));
#7415=DIRECTION('',(0.,1.,0.));
#7416=DIRECTION('',(-1.,0.,0.));
#7417=DIRECTION('',(0.,-1.,0.));
#7418=DIRECTION('',(1.,0.,0.));
#7419=DIRECTION('',(0.,1.,0.));
#7420=DIRECTION('',(-1.,0.,0.));
#7421=DIRECTION('',(0.,-1.,0.));
#7422=DIRECTION('',(1.,0.,0.));
#7423=DIRECTION('',(0.,1.,0.));
#7424=DIRECTION('',(-1.,0.,0.));
#7425=DIRECTION('',(0.,-1.,0.));
#7426=DIRECTION('center_axis',(0.,0.,-1.));
#7427=DIRECTION('ref_axis',(1.,-4.37659398927547E-14,0.));
#7428=DIRECTION('center_axis',(0.,0.,-1.));
#7429=DIRECTION('ref_axis',(1.,-4.2144979155986E-14,0.));
#7430=DIRECTION('center_axis',(0.,0.,-1.));
#7431=DIRECTION('ref_axis',(1.,-4.32256196471651E-14,0.));
#7432=DIRECTION('center_axis',(0.,0.,1.));
#7433=DIRECTION('ref_axis',(1.,0.,0.));
#7434=DIRECTION('',(-1.,0.,0.));
#7435=DIRECTION('',(-0.707106781186548,-0.707106781186547,0.));
#7436=DIRECTION('',(0.,-1.,0.));
#7437=DIRECTION('',(-1.,0.,0.));
#7438=DIRECTION('',(0.,1.,0.));
#7439=DIRECTION('',(1.,0.,0.));
#7440=DIRECTION('',(0.,-1.,0.));
#7441=DIRECTION('',(-1.,0.,0.));
#7442=DIRECTION('',(0.,1.,0.));
#7443=DIRECTION('',(1.,0.,0.));
#7444=DIRECTION('',(0.,-1.,0.));
#7445=DIRECTION('',(-1.,0.,0.));
#7446=DIRECTION('',(0.,1.,0.));
#7447=DIRECTION('',(1.,0.,0.));
#7448=DIRECTION('',(0.,-1.,0.));
#7449=DIRECTION('center_axis',(0.,0.,1.));
#7450=DIRECTION('ref_axis',(-1.,0.,0.));
#7451=DIRECTION('center_axis',(0.,0.,-1.));
#7452=DIRECTION('ref_axis',(1.,0.,0.));
#7453=DIRECTION('center_axis',(0.,0.,1.));
#7454=DIRECTION('ref_axis',(-1.,0.,0.));
#7455=DIRECTION('',(0.,-1.,0.));
#7456=DIRECTION('center_axis',(0.,0.,-1.));
#7457=DIRECTION('ref_axis',(1.,0.,0.));
#7458=DIRECTION('center_axis',(0.,0.,-1.));
#7459=DIRECTION('ref_axis',(1.,0.,0.));
#7460=DIRECTION('center_axis',(0.,0.,1.));
#7461=DIRECTION('ref_axis',(-1.,0.,0.));
#7462=DIRECTION('center_axis',(0.,0.,-1.));
#7463=DIRECTION('ref_axis',(1.,0.,0.));
#7464=DIRECTION('center_axis',(0.,0.,1.));
#7465=DIRECTION('ref_axis',(-1.,0.,0.));
#7466=DIRECTION('center_axis',(0.,-1.,0.));
#7467=DIRECTION('ref_axis',(-1.,0.,0.));
#7468=DIRECTION('',(0.,0.,-1.));
#7469=DIRECTION('',(0.,0.,-1.));
#7470=DIRECTION('center_axis',(1.,0.,0.));
#7471=DIRECTION('ref_axis',(0.,-1.,0.));
#7472=DIRECTION('',(0.,0.,-1.));
#7473=DIRECTION('center_axis',(0.,1.,0.));
#7474=DIRECTION('ref_axis',(1.,0.,0.));
#7475=DIRECTION('',(0.,0.,-1.));
#7476=DIRECTION('center_axis',(-1.,0.,0.));
#7477=DIRECTION('ref_axis',(0.,1.,0.));
#7478=DIRECTION('center_axis',(0.,-1.,0.));
#7479=DIRECTION('ref_axis',(-1.,0.,0.));
#7480=DIRECTION('',(0.,0.,-1.));
#7481=DIRECTION('',(0.,0.,-1.));
#7482=DIRECTION('center_axis',(1.,0.,0.));
#7483=DIRECTION('ref_axis',(0.,-1.,0.));
#7484=DIRECTION('',(0.,0.,-1.));
#7485=DIRECTION('center_axis',(0.,1.,0.));
#7486=DIRECTION('ref_axis',(1.,0.,0.));
#7487=DIRECTION('',(0.,0.,-1.));
#7488=DIRECTION('center_axis',(-1.,0.,0.));
#7489=DIRECTION('ref_axis',(0.,1.,0.));
#7490=DIRECTION('center_axis',(0.,-1.,0.));
#7491=DIRECTION('ref_axis',(-1.,0.,0.));
#7492=DIRECTION('',(0.,0.,-1.));
#7493=DIRECTION('',(0.,0.,-1.));
#7494=DIRECTION('center_axis',(1.,0.,0.));
#7495=DIRECTION('ref_axis',(0.,-1.,0.));
#7496=DIRECTION('',(0.,0.,-1.));
#7497=DIRECTION('center_axis',(0.,1.,0.));
#7498=DIRECTION('ref_axis',(1.,0.,0.));
#7499=DIRECTION('',(0.,0.,-1.));
#7500=DIRECTION('center_axis',(-1.,0.,0.));
#7501=DIRECTION('ref_axis',(0.,1.,0.));
#7502=DIRECTION('center_axis',(0.,0.,1.));
#7503=DIRECTION('ref_axis',(1.,0.,0.));
#7504=DIRECTION('',(0.,-1.,0.));
#7505=DIRECTION('',(1.,0.,0.));
#7506=DIRECTION('',(0.707106781186548,0.707106781186548,0.));
#7507=DIRECTION('',(0.,1.,0.));
#7508=DIRECTION('',(-1.,0.,0.));
#7509=DIRECTION('',(0.,-1.,0.));
#7510=DIRECTION('',(0.707106781186548,-0.707106781186548,0.));
#7511=DIRECTION('',(1.,0.,0.));
#7512=DIRECTION('center_axis',(0.,-1.,0.));
#7513=DIRECTION('ref_axis',(1.,0.,0.));
#7514=DIRECTION('',(0.,0.,1.));
#7515=DIRECTION('center_axis',(-1.,0.,0.));
#7516=DIRECTION('ref_axis',(0.,-1.,0.));
#7517=DIRECTION('center_axis',(0.,-1.,0.));
#7518=DIRECTION('ref_axis',(1.,0.,0.));
#7519=DIRECTION('',(0.,0.,1.));
#7520=DIRECTION('center_axis',(0.707106781186547,-0.707106781186548,0.));
#7521=DIRECTION('ref_axis',(0.707106781186548,0.707106781186547,0.));
#7522=DIRECTION('',(0.,0.,1.));
#7523=DIRECTION('center_axis',(1.,0.,0.));
#7524=DIRECTION('ref_axis',(0.,1.,0.));
#7525=DIRECTION('',(0.,0.,1.));
#7526=DIRECTION('',(0.,0.,1.));
#7527=DIRECTION('center_axis',(0.,-1.,0.));
#7528=DIRECTION('ref_axis',(1.,0.,0.));
#7529=DIRECTION('',(0.,0.,1.));
#7530=DIRECTION('center_axis',(-1.,0.,0.));
#7531=DIRECTION('ref_axis',(0.,-1.,0.));
#7532=DIRECTION('',(0.,0.,1.));
#7533=DIRECTION('center_axis',(1.,0.,0.));
#7534=DIRECTION('ref_axis',(0.,1.,0.));
#7535=DIRECTION('center_axis',(-0.707106781186548,0.707106781186548,0.));
#7536=DIRECTION('ref_axis',(-0.707106781186548,-0.707106781186548,0.));
#7537=DIRECTION('',(0.,0.,1.));
#7538=DIRECTION('center_axis',(0.,1.,0.));
#7539=DIRECTION('ref_axis',(-1.,0.,0.));
#7540=DIRECTION('',(0.,0.,1.));
#7541=DIRECTION('center_axis',(0.707106781186548,0.707106781186548,0.));
#7542=DIRECTION('ref_axis',(-0.707106781186548,0.707106781186548,0.));
#7543=DIRECTION('axis',(0.,0.,1.));
#7544=DIRECTION('refdir',(1.,0.,0.));
#7545=DIRECTION('center_axis',(0.408248290463861,-0.816496580927726,0.408248290463864));
#7546=DIRECTION('ref_axis',(0.577350269189625,0.577350269189625,0.577350269189629));
#7547=DIRECTION('center_axis',(0.,1.,4.44089209850063E-15));
#7548=DIRECTION('ref_axis',(1.,0.,0.));
#7549=DIRECTION('center_axis',(0.,0.,1.));
#7550=DIRECTION('ref_axis',(0.,1.,0.));
#7551=DIRECTION('center_axis',(1.,-4.44089209850062E-15,0.));
#7552=DIRECTION('ref_axis',(0.,0.,1.));
#7553=DIRECTION('center_axis',(-0.40824829046386,-0.816496580927728,0.408248290463862));
#7554=DIRECTION('ref_axis',(-0.577350269189625,0.577350269189625,0.577350269189628));
#7555=DIRECTION('center_axis',(-1.,0.,0.));
#7556=DIRECTION('ref_axis',(0.,1.,0.));
#7557=DIRECTION('center_axis',(0.,0.,1.));
#7558=DIRECTION('ref_axis',(-1.,0.,0.));
#7559=DIRECTION('center_axis',(4.44089209850062E-15,1.,0.));
#7560=DIRECTION('ref_axis',(0.,0.,1.));
#7561=DIRECTION('center_axis',(-0.816496580927725,0.408248290463866,-0.408248290463862));
#7562=DIRECTION('ref_axis',(0.577350269189629,0.577350269189625,-0.577350269189623));
#7563=DIRECTION('center_axis',(0.,0.,-1.));
#7564=DIRECTION('ref_axis',(1.,0.,0.));
#7565=DIRECTION('center_axis',(-4.44089209850062E-15,1.,0.));
#7566=DIRECTION('ref_axis',(0.,0.,-1.));
#7567=DIRECTION('center_axis',(1.,0.,-4.44089209850063E-15));
#7568=DIRECTION('ref_axis',(0.,1.,0.));
#7569=DIRECTION('center_axis',(-0.408248290463861,-0.816496580927728,-0.408248290463861));
#7570=DIRECTION('ref_axis',(0.577350269189625,-0.577350269189625,0.577350269189628));
#7571=DIRECTION('center_axis',(1.,0.,0.));
#7572=DIRECTION('ref_axis',(0.,-1.,0.));
#7573=DIRECTION('center_axis',(0.,0.,1.));
#7574=DIRECTION('ref_axis',(1.,0.,0.));
#7575=DIRECTION('center_axis',(-4.44089209850062E-15,-1.,0.));
#7576=DIRECTION('ref_axis',(0.,0.,1.));
#7577=DIRECTION('center_axis',(0.408248290463867,-0.408248290463859,-0.816496580927726));
#7578=DIRECTION('ref_axis',(-0.577350269189629,0.577350269189622,-0.577350269189626));
#7579=DIRECTION('center_axis',(-1.,0.,0.));
#7580=DIRECTION('ref_axis',(0.,0.,-1.));
#7581=DIRECTION('center_axis',(0.,1.,-4.44089209850063E-15));
#7582=DIRECTION('ref_axis',(-1.,0.,0.));
#7583=DIRECTION('center_axis',(0.,0.,-1.));
#7584=DIRECTION('ref_axis',(0.,1.,0.));
#7585=DIRECTION('center_axis',(0.408248290463861,-0.816496580927726,-0.408248290463864));
#7586=DIRECTION('ref_axis',(-0.577350269189625,-0.577350269189625,0.577350269189629));
#7587=DIRECTION('center_axis',(0.,-1.,4.44089209850063E-15));
#7588=DIRECTION('ref_axis',(-1.,0.,0.));
#7589=DIRECTION('center_axis',(0.,0.,1.));
#7590=DIRECTION('ref_axis',(0.,-1.,0.));
#7591=DIRECTION('center_axis',(-1.,4.44089209850062E-15,0.));
#7592=DIRECTION('ref_axis',(0.,0.,1.));
#7593=DIRECTION('center_axis',(-0.816496580927729,-0.408248290463861,-0.40824829046386));
#7594=DIRECTION('ref_axis',(0.577350269189622,-0.577350269189629,-0.577350269189626));
#7595=DIRECTION('center_axis',(0.,0.,-1.));
#7596=DIRECTION('ref_axis',(0.,-1.,0.));
#7597=DIRECTION('center_axis',(1.,0.,0.));
#7598=DIRECTION('ref_axis',(0.,0.,-1.));
#7599=DIRECTION('center_axis',(0.,-1.,-4.44089209850063E-15));
#7600=DIRECTION('ref_axis',(1.,0.,0.));
#7601=DIRECTION('center_axis',(-0.816496580927726,0.408248290463863,0.408248290463863));
#7602=DIRECTION('ref_axis',(-0.577350269189629,-0.577350269189625,-0.577350269189623));
#7603=DIRECTION('center_axis',(0.,0.,-1.));
#7604=DIRECTION('ref_axis',(-1.,0.,0.));
#7605=DIRECTION('center_axis',(4.44089209850062E-15,-1.,0.));
#7606=DIRECTION('ref_axis',(0.,0.,-1.));
#7607=DIRECTION('center_axis',(-1.,0.,-4.44089209850063E-15));
#7608=DIRECTION('ref_axis',(0.,-1.,0.));
#7609=DIRECTION('center_axis',(0.,-1.,0.));
#7610=DIRECTION('ref_axis',(-0.707106781186549,0.,-0.707106781186546));
#7611=DIRECTION('',(0.,1.,0.));
#7612=DIRECTION('',(0.,-1.,0.));
#7613=DIRECTION('center_axis',(1.,0.,0.));
#7614=DIRECTION('ref_axis',(0.,-0.707106781186549,-0.707106781186546));
#7615=DIRECTION('',(-1.,0.,0.));
#7616=DIRECTION('',(1.,0.,0.));
#7617=DIRECTION('center_axis',(0.,0.,1.));
#7618=DIRECTION('ref_axis',(-0.707106781186548,-0.707106781186548,0.));
#7619=DIRECTION('',(0.,0.,-1.));
#7620=DIRECTION('',(0.,0.,1.));
#7621=DIRECTION('center_axis',(0.,1.,0.));
#7622=DIRECTION('ref_axis',(0.707106781186549,0.,-0.707106781186546));
#7623=DIRECTION('',(0.,-1.,0.));
#7624=DIRECTION('',(0.,1.,0.));
#7625=DIRECTION('center_axis',(0.,0.,1.));
#7626=DIRECTION('ref_axis',(0.707106781186548,-0.707106781186548,0.));
#7627=DIRECTION('',(0.,0.,-1.));
#7628=DIRECTION('',(0.,0.,1.));
#7629=DIRECTION('center_axis',(1.,0.,0.));
#7630=DIRECTION('ref_axis',(0.,-0.707106781186549,0.707106781186546));
#7631=DIRECTION('',(-1.,0.,0.));
#7632=DIRECTION('',(1.,0.,0.));
#7633=DIRECTION('center_axis',(0.,-1.,0.));
#7634=DIRECTION('ref_axis',(-0.707106781186549,0.,0.707106781186546));
#7635=DIRECTION('',(0.,1.,0.));
#7636=DIRECTION('',(0.,-1.,0.));
#7637=DIRECTION('center_axis',(0.,0.,1.));
#7638=DIRECTION('ref_axis',(-0.707106781186548,0.707106781186548,0.));
#7639=DIRECTION('',(0.,0.,-1.));
#7640=DIRECTION('',(0.,0.,1.));
#7641=DIRECTION('center_axis',(-1.,0.,0.));
#7642=DIRECTION('ref_axis',(0.,0.707106781186549,-0.707106781186546));
#7643=DIRECTION('',(1.,0.,0.));
#7644=DIRECTION('',(-1.,0.,0.));
#7645=DIRECTION('center_axis',(0.,1.,0.));
#7646=DIRECTION('ref_axis',(0.707106781186549,0.,0.707106781186546));
#7647=DIRECTION('',(0.,-1.,0.));
#7648=DIRECTION('',(0.,1.,0.));
#7649=DIRECTION('center_axis',(0.,0.,1.));
#7650=DIRECTION('ref_axis',(0.707106781186548,0.707106781186548,0.));
#7651=DIRECTION('',(0.,0.,-1.));
#7652=DIRECTION('',(0.,0.,1.));
#7653=DIRECTION('center_axis',(-1.,0.,0.));
#7654=DIRECTION('ref_axis',(0.,0.707106781186549,0.707106781186546));
#7655=DIRECTION('',(1.,0.,0.));
#7656=DIRECTION('',(-1.,0.,0.));
#7657=DIRECTION('center_axis',(-1.,0.,0.));
#7658=DIRECTION('ref_axis',(0.,-1.,0.));
#7659=DIRECTION('center_axis',(0.,0.,1.));
#7660=DIRECTION('ref_axis',(1.,0.,0.));
#7661=DIRECTION('',(1.,0.,0.));
#7662=DIRECTION('',(0.,1.,0.));
#7663=DIRECTION('',(-1.,0.,0.));
#7664=DIRECTION('',(0.,-1.,0.));
#7665=DIRECTION('center_axis',(0.,0.,1.));
#7666=DIRECTION('ref_axis',(1.,0.,0.));
#7667=DIRECTION('center_axis',(0.,0.,1.));
#7668=DIRECTION('ref_axis',(1.,0.,0.));
#7669=DIRECTION('center_axis',(0.,-1.,0.));
#7670=DIRECTION('ref_axis',(1.,0.,0.));
#7671=DIRECTION('center_axis',(1.,0.,0.));
#7672=DIRECTION('ref_axis',(0.,1.,0.));
#7673=DIRECTION('center_axis',(0.,0.,1.));
#7674=DIRECTION('ref_axis',(1.,0.,0.));
#7675=DIRECTION('',(-1.,0.,0.));
#7676=DIRECTION('',(0.,1.,0.));
#7677=DIRECTION('',(1.,0.,0.));
#7678=DIRECTION('',(0.,-1.,0.));
#7679=DIRECTION('center_axis',(0.,0.,-1.));
#7680=DIRECTION('ref_axis',(1.,0.,0.));
#7681=DIRECTION('center_axis',(0.,0.,-1.));
#7682=DIRECTION('ref_axis',(1.,0.,0.));
#7683=DIRECTION('center_axis',(0.,1.,0.));
#7684=DIRECTION('ref_axis',(-1.,0.,0.));
#7685=DIRECTION('center_axis',(0.,0.,-1.));
#7686=DIRECTION('ref_axis',(1.,0.,0.));
#7687=DIRECTION('',(0.,0.,-1.));
#7688=DIRECTION('center_axis',(0.,0.,-1.));
#7689=DIRECTION('ref_axis',(1.,0.,0.));
#7690=DIRECTION('',(0.,0.,-1.));
#7691=DIRECTION('center_axis',(0.,-1.,0.));
#7692=DIRECTION('ref_axis',(-1.,0.,0.));
#7693=DIRECTION('',(0.,0.,-1.));
#7694=DIRECTION('',(0.,0.,-1.));
#7695=DIRECTION('center_axis',(1.,0.,0.));
#7696=DIRECTION('ref_axis',(0.,-1.,0.));
#7697=DIRECTION('',(0.,0.,-1.));
#7698=DIRECTION('center_axis',(0.,1.,0.));
#7699=DIRECTION('ref_axis',(1.,0.,0.));
#7700=DIRECTION('',(0.,0.,-1.));
#7701=DIRECTION('center_axis',(-1.,0.,0.));
#7702=DIRECTION('ref_axis',(0.,1.,0.));
#7703=DIRECTION('axis',(0.,0.,1.));
#7704=DIRECTION('refdir',(1.,0.,0.));
#7705=DIRECTION('center_axis',(0.,0.,-1.));
#7706=DIRECTION('ref_axis',(1.,0.,0.));
#7707=DIRECTION('center_axis',(0.,0.,-1.));
#7708=DIRECTION('ref_axis',(1.,0.,0.));
#7709=DIRECTION('',(0.,0.,-1.));
#7710=DIRECTION('center_axis',(0.,0.,1.));
#7711=DIRECTION('ref_axis',(1.,0.,0.));
#7712=DIRECTION('center_axis',(0.,0.,-1.));
#7713=DIRECTION('ref_axis',(1.,0.,0.));
#7714=DIRECTION('center_axis',(0.,0.,-1.));
#7715=DIRECTION('ref_axis',(1.,0.,0.));
#7716=DIRECTION('',(0.,0.,-1.));
#7717=DIRECTION('center_axis',(0.,0.,1.));
#7718=DIRECTION('ref_axis',(1.,0.,0.));
#7719=DIRECTION('center_axis',(0.,1.,0.));
#7720=DIRECTION('ref_axis',(-1.,0.,0.));
#7721=DIRECTION('',(-1.,0.,0.));
#7722=DIRECTION('',(0.,0.,1.));
#7723=DIRECTION('',(-1.,0.,0.));
#7724=DIRECTION('',(0.,0.,1.));
#7725=DIRECTION('center_axis',(-1.,0.,0.));
#7726=DIRECTION('ref_axis',(0.,-1.,0.));
#7727=DIRECTION('',(0.,-1.,0.));
#7728=DIRECTION('',(0.,-1.,0.));
#7729=DIRECTION('',(0.,0.,1.));
#7730=DIRECTION('center_axis',(0.,-1.,0.));
#7731=DIRECTION('ref_axis',(1.,0.,0.));
#7732=DIRECTION('',(1.,0.,0.));
#7733=DIRECTION('',(1.,0.,0.));
#7734=DIRECTION('',(0.,0.,1.));
#7735=DIRECTION('center_axis',(1.,0.,0.));
#7736=DIRECTION('ref_axis',(0.,1.,0.));
#7737=DIRECTION('',(0.,1.,0.));
#7738=DIRECTION('',(0.,1.,0.));
#7739=DIRECTION('center_axis',(0.,1.,0.));
#7740=DIRECTION('ref_axis',(-1.,0.,0.));
#7741=DIRECTION('',(-1.,0.,0.));
#7742=DIRECTION('',(0.,0.,1.));
#7743=DIRECTION('',(-1.,0.,0.));
#7744=DIRECTION('',(0.,0.,1.));
#7745=DIRECTION('center_axis',(1.,0.,0.));
#7746=DIRECTION('ref_axis',(0.,1.,0.));
#7747=DIRECTION('',(0.,1.,0.));
#7748=DIRECTION('',(0.,1.,0.));
#7749=DIRECTION('',(0.,0.,1.));
#7750=DIRECTION('center_axis',(0.,-1.,0.));
#7751=DIRECTION('ref_axis',(1.,0.,0.));
#7752=DIRECTION('',(1.,0.,0.));
#7753=DIRECTION('',(1.,0.,0.));
#7754=DIRECTION('',(0.,0.,1.));
#7755=DIRECTION('center_axis',(-1.,0.,0.));
#7756=DIRECTION('ref_axis',(0.,-1.,0.));
#7757=DIRECTION('',(0.,-1.,0.));
#7758=DIRECTION('',(0.,-1.,0.));
#7759=DIRECTION('center_axis',(0.,0.,1.));
#7760=DIRECTION('ref_axis',(1.,0.,0.));
#7761=DIRECTION('center_axis',(0.,0.,1.));
#7762=DIRECTION('ref_axis',(1.,0.,0.));
#7763=DIRECTION('axis',(0.,0.,1.));
#7764=DIRECTION('refdir',(1.,0.,0.));
#7765=DIRECTION('center_axis',(0.,0.,-1.));
#7766=DIRECTION('ref_axis',(1.,0.,0.));
#7767=DIRECTION('center_axis',(0.,0.,-1.));
#7768=DIRECTION('ref_axis',(1.,0.,0.));
#7769=DIRECTION('',(0.,0.,-1.));
#7770=DIRECTION('center_axis',(0.,0.,1.));
#7771=DIRECTION('ref_axis',(1.,0.,0.));
#7772=DIRECTION('center_axis',(0.,0.,-1.));
#7773=DIRECTION('ref_axis',(1.,0.,0.));
#7774=DIRECTION('center_axis',(0.,0.,-1.));
#7775=DIRECTION('ref_axis',(1.,0.,0.));
#7776=DIRECTION('',(0.,0.,-1.));
#7777=DIRECTION('center_axis',(0.,0.,1.));
#7778=DIRECTION('ref_axis',(1.,0.,0.));
#7779=DIRECTION('center_axis',(0.,0.,-1.));
#7780=DIRECTION('ref_axis',(1.,0.,0.));
#7781=DIRECTION('center_axis',(0.,0.,-1.));
#7782=DIRECTION('ref_axis',(1.,0.,0.));
#7783=DIRECTION('',(0.,0.,-1.));
#7784=DIRECTION('center_axis',(0.,0.,1.));
#7785=DIRECTION('ref_axis',(1.,0.,0.));
#7786=DIRECTION('center_axis',(0.,0.,-1.));
#7787=DIRECTION('ref_axis',(1.,0.,0.));
#7788=DIRECTION('center_axis',(0.,0.,-1.));
#7789=DIRECTION('ref_axis',(1.,0.,0.));
#7790=DIRECTION('',(0.,0.,-1.));
#7791=DIRECTION('center_axis',(0.,0.,1.));
#7792=DIRECTION('ref_axis',(1.,0.,0.));
#7793=DIRECTION('center_axis',(0.,-1.,0.));
#7794=DIRECTION('ref_axis',(-1.,0.,0.));
#7795=DIRECTION('',(-1.,0.,0.));
#7796=DIRECTION('',(0.,0.,-1.));
#7797=DIRECTION('',(1.,0.,0.));
#7798=DIRECTION('',(0.,0.,-1.));
#7799=DIRECTION('center_axis',(1.,0.,0.));
#7800=DIRECTION('ref_axis',(0.,-1.,0.));
#7801=DIRECTION('',(0.,-1.,0.));
#7802=DIRECTION('',(0.,0.,-1.));
#7803=DIRECTION('',(0.,1.,0.));
#7804=DIRECTION('center_axis',(0.,1.,0.));
#7805=DIRECTION('ref_axis',(1.,0.,0.));
#7806=DIRECTION('',(1.,0.,0.));
#7807=DIRECTION('',(0.,0.,-1.));
#7808=DIRECTION('',(-1.,0.,0.));
#7809=DIRECTION('center_axis',(-1.,0.,0.));
#7810=DIRECTION('ref_axis',(0.,1.,0.));
#7811=DIRECTION('',(0.,1.,0.));
#7812=DIRECTION('',(0.,-1.,0.));
#7813=DIRECTION('center_axis',(0.,-1.,0.));
#7814=DIRECTION('ref_axis',(-1.,0.,0.));
#7815=DIRECTION('',(-1.,0.,0.));
#7816=DIRECTION('',(0.,0.,-1.));
#7817=DIRECTION('',(1.,0.,0.));
#7818=DIRECTION('',(0.,0.,-1.));
#7819=DIRECTION('center_axis',(1.,0.,0.));
#7820=DIRECTION('ref_axis',(0.,-1.,0.));
#7821=DIRECTION('',(0.,-1.,0.));
#7822=DIRECTION('',(0.,0.,-1.));
#7823=DIRECTION('',(0.,1.,0.));
#7824=DIRECTION('center_axis',(0.,1.,0.));
#7825=DIRECTION('ref_axis',(1.,0.,0.));
#7826=DIRECTION('',(1.,0.,0.));
#7827=DIRECTION('',(0.,0.,-1.));
#7828=DIRECTION('',(-1.,0.,0.));
#7829=DIRECTION('center_axis',(-1.,0.,0.));
#7830=DIRECTION('ref_axis',(0.,1.,0.));
#7831=DIRECTION('',(0.,1.,0.));
#7832=DIRECTION('',(0.,-1.,0.));
#7833=DIRECTION('center_axis',(0.,-1.,0.));
#7834=DIRECTION('ref_axis',(-1.,0.,0.));
#7835=DIRECTION('',(-1.,0.,0.));
#7836=DIRECTION('',(0.,0.,-1.));
#7837=DIRECTION('',(1.,0.,0.));
#7838=DIRECTION('',(0.,0.,-1.));
#7839=DIRECTION('center_axis',(1.,0.,0.));
#7840=DIRECTION('ref_axis',(0.,-1.,0.));
#7841=DIRECTION('',(0.,-1.,0.));
#7842=DIRECTION('',(0.,0.,-1.));
#7843=DIRECTION('',(0.,1.,0.));
#7844=DIRECTION('center_axis',(0.,1.,0.));
#7845=DIRECTION('ref_axis',(1.,0.,0.));
#7846=DIRECTION('',(1.,0.,0.));
#7847=DIRECTION('',(0.,0.,-1.));
#7848=DIRECTION('',(-1.,0.,0.));
#7849=DIRECTION('center_axis',(-1.,0.,0.));
#7850=DIRECTION('ref_axis',(0.,1.,0.));
#7851=DIRECTION('',(0.,1.,0.));
#7852=DIRECTION('',(0.,-1.,0.));
#7853=DIRECTION('center_axis',(0.,1.,0.));
#7854=DIRECTION('ref_axis',(-1.,0.,0.));
#7855=DIRECTION('',(-1.,0.,0.));
#7856=DIRECTION('',(0.,0.,1.));
#7857=DIRECTION('',(-1.,0.,0.));
#7858=DIRECTION('',(0.,0.,1.));
#7859=DIRECTION('center_axis',(1.,0.,0.));
#7860=DIRECTION('ref_axis',(0.,1.,0.));
#7861=DIRECTION('',(0.,1.,0.));
#7862=DIRECTION('',(0.,1.,0.));
#7863=DIRECTION('',(0.,0.,1.));
#7864=DIRECTION('center_axis',(0.,-1.,0.));
#7865=DIRECTION('ref_axis',(1.,0.,0.));
#7866=DIRECTION('',(1.,0.,0.));
#7867=DIRECTION('',(1.,0.,0.));
#7868=DIRECTION('',(0.,0.,1.));
#7869=DIRECTION('center_axis',(-1.,0.,0.));
#7870=DIRECTION('ref_axis',(0.,-1.,0.));
#7871=DIRECTION('',(0.,-1.,0.));
#7872=DIRECTION('',(0.,-1.,0.));
#7873=DIRECTION('center_axis',(0.,0.,1.));
#7874=DIRECTION('ref_axis',(1.,0.,0.));
#7875=DIRECTION('center_axis',(0.,0.,1.));
#7876=DIRECTION('ref_axis',(1.,0.,0.));
#7877=DIRECTION('axis',(0.,0.,1.));
#7878=DIRECTION('refdir',(1.,0.,0.));
#7879=DIRECTION('center_axis',(0.,-1.,0.));
#7880=DIRECTION('ref_axis',(0.,0.,1.));
#7881=DIRECTION('center_axis',(0.,-1.,0.));
#7882=DIRECTION('ref_axis',(0.,0.,1.));
#7883=DIRECTION('',(0.,-1.,0.));
#7884=DIRECTION('center_axis',(0.,1.,0.));
#7885=DIRECTION('ref_axis',(0.,0.,1.));
#7886=DIRECTION('center_axis',(0.,1.,0.));
#7887=DIRECTION('ref_axis',(-1.,0.,0.));
#7888=DIRECTION('',(-1.,0.,0.));
#7889=DIRECTION('',(0.,0.,1.));
#7890=DIRECTION('',(-1.,0.,0.));
#7891=DIRECTION('',(0.,0.,1.));
#7892=DIRECTION('center_axis',(1.,0.,0.));
#7893=DIRECTION('ref_axis',(0.,1.,0.));
#7894=DIRECTION('',(0.,1.,0.));
#7895=DIRECTION('',(0.,1.,0.));
#7896=DIRECTION('',(0.,0.,1.));
#7897=DIRECTION('center_axis',(0.,-1.,0.));
#7898=DIRECTION('ref_axis',(1.,0.,0.));
#7899=DIRECTION('',(1.,0.,0.));
#7900=DIRECTION('',(1.,0.,0.));
#7901=DIRECTION('',(0.,0.,1.));
#7902=DIRECTION('center_axis',(-1.,0.,0.));
#7903=DIRECTION('ref_axis',(0.,-1.,0.));
#7904=DIRECTION('',(0.,-1.,0.));
#7905=DIRECTION('',(0.,-1.,0.));
#7906=DIRECTION('center_axis',(0.,0.,1.));
#7907=DIRECTION('ref_axis',(1.,0.,0.));
#7908=DIRECTION('center_axis',(0.,0.,1.));
#7909=DIRECTION('ref_axis',(1.,0.,0.));
#7910=DIRECTION('axis',(0.,0.,1.));
#7911=DIRECTION('refdir',(1.,0.,0.));
#7912=DIRECTION('center_axis',(0.,-1.,0.));
#7913=DIRECTION('ref_axis',(0.,0.,1.));
#7914=DIRECTION('center_axis',(0.,-1.,0.));
#7915=DIRECTION('ref_axis',(0.,0.,1.));
#7916=DIRECTION('',(0.,-1.,0.));
#7917=DIRECTION('center_axis',(0.,1.,0.));
#7918=DIRECTION('ref_axis',(0.,0.,1.));
#7919=DIRECTION('center_axis',(0.,1.,0.));
#7920=DIRECTION('ref_axis',(-1.,0.,0.));
#7921=DIRECTION('',(-1.,0.,0.));
#7922=DIRECTION('',(0.,0.,1.));
#7923=DIRECTION('',(-1.,0.,0.));
#7924=DIRECTION('',(0.,0.,1.));
#7925=DIRECTION('center_axis',(1.,0.,0.));
#7926=DIRECTION('ref_axis',(0.,1.,0.));
#7927=DIRECTION('',(0.,1.,0.));
#7928=DIRECTION('',(0.,1.,0.));
#7929=DIRECTION('',(0.,0.,1.));
#7930=DIRECTION('center_axis',(0.,-1.,0.));
#7931=DIRECTION('ref_axis',(1.,0.,0.));
#7932=DIRECTION('',(1.,0.,0.));
#7933=DIRECTION('',(1.,0.,0.));
#7934=DIRECTION('',(0.,0.,1.));
#7935=DIRECTION('center_axis',(-1.,0.,0.));
#7936=DIRECTION('ref_axis',(0.,-1.,0.));
#7937=DIRECTION('',(0.,-1.,0.));
#7938=DIRECTION('',(0.,-1.,0.));
#7939=DIRECTION('center_axis',(0.,0.,1.));
#7940=DIRECTION('ref_axis',(1.,0.,0.));
#7941=DIRECTION('center_axis',(0.,0.,1.));
#7942=DIRECTION('ref_axis',(1.,0.,0.));
#7943=DIRECTION('axis',(0.,0.,1.));
#7944=DIRECTION('refdir',(1.,0.,0.));
#7945=DIRECTION('center_axis',(0.,0.,1.));
#7946=DIRECTION('ref_axis',(1.,0.,0.));
#7947=DIRECTION('',(0.,0.,-1.));
#7948=DIRECTION('center_axis',(0.,0.,-1.));
#7949=DIRECTION('ref_axis',(1.,0.,0.));
#7950=DIRECTION('center_axis',(0.,0.,1.));
#7951=DIRECTION('ref_axis',(1.,0.,0.));
#7952=DIRECTION('',(0.,0.,-1.));
#7953=DIRECTION('center_axis',(0.,0.,1.));
#7954=DIRECTION('ref_axis',(1.,0.,0.));
#7955=DIRECTION('',(0.,0.,-1.));
#7956=DIRECTION('center_axis',(0.,0.,1.));
#7957=DIRECTION('ref_axis',(1.,0.,0.));
#7958=DIRECTION('',(0.,0.,-1.));
#7959=DIRECTION('center_axis',(0.,0.,1.));
#7960=DIRECTION('ref_axis',(1.,0.,0.));
#7961=DIRECTION('',(0.,0.,-1.));
#7962=DIRECTION('center_axis',(0.,0.,1.));
#7963=DIRECTION('ref_axis',(1.,0.,0.));
#7964=DIRECTION('',(0.,0.,-1.));
#7965=DIRECTION('center_axis',(0.,0.,1.));
#7966=DIRECTION('ref_axis',(1.,0.,0.));
#7967=DIRECTION('',(0.,0.,-1.));
#7968=DIRECTION('center_axis',(0.,0.,1.));
#7969=DIRECTION('ref_axis',(1.,0.,0.));
#7970=DIRECTION('',(0.,0.,-1.));
#7971=DIRECTION('center_axis',(0.,0.,1.));
#7972=DIRECTION('ref_axis',(1.,0.,0.));
#7973=DIRECTION('',(0.,0.,-1.));
#7974=DIRECTION('center_axis',(0.,0.,1.));
#7975=DIRECTION('ref_axis',(1.,0.,0.));
#7976=DIRECTION('',(0.,0.,-1.));
#7977=DIRECTION('center_axis',(0.,0.,1.));
#7978=DIRECTION('ref_axis',(0.99867308056793,-0.051498331516286,0.));
#7979=DIRECTION('',(0.,0.,1.));
#7980=DIRECTION('center_axis',(0.,0.,-1.));
#7981=DIRECTION('ref_axis',(1.,5.83250561478606E-14,0.));
#7982=DIRECTION('center_axis',(0.,0.,1.));
#7983=DIRECTION('ref_axis',(1.,5.83250561478606E-14,0.));
#7984=DIRECTION('',(0.,0.,1.));
#7985=DIRECTION('center_axis',(0.,0.,1.));
#7986=DIRECTION('ref_axis',(1.,5.83250561478606E-14,0.));
#7987=DIRECTION('',(0.,0.,1.));
#7988=DIRECTION('center_axis',(0.,0.,1.));
#7989=DIRECTION('ref_axis',(1.,5.83250561478606E-14,0.));
#7990=DIRECTION('',(0.,0.,1.));
#7991=DIRECTION('center_axis',(0.,0.,1.));
#7992=DIRECTION('ref_axis',(1.,5.83250561478606E-14,0.));
#7993=DIRECTION('',(0.,0.,1.));
#7994=DIRECTION('center_axis',(0.,0.,1.));
#7995=DIRECTION('ref_axis',(1.,5.83250561478606E-14,0.));
#7996=DIRECTION('',(0.,0.,1.));
#7997=DIRECTION('center_axis',(0.,0.,1.));
#7998=DIRECTION('ref_axis',(1.,5.83250561478606E-14,0.));
#7999=DIRECTION('',(0.,0.,1.));
#8000=DIRECTION('center_axis',(0.,0.,1.));
#8001=DIRECTION('ref_axis',(1.,5.83250561478606E-14,0.));
#8002=DIRECTION('',(0.,0.,1.));
#8003=DIRECTION('center_axis',(0.,0.,1.));
#8004=DIRECTION('ref_axis',(1.,5.83250561478606E-14,0.));
#8005=DIRECTION('',(0.,0.,1.));
#8006=DIRECTION('center_axis',(0.,0.,1.));
#8007=DIRECTION('ref_axis',(1.,5.83250561478606E-14,0.));
#8008=DIRECTION('',(0.,0.,1.));
#8009=DIRECTION('center_axis',(0.,0.,-1.));
#8010=DIRECTION('ref_axis',(1.,0.,0.));
#8011=DIRECTION('center_axis',(0.,0.,-1.));
#8012=DIRECTION('ref_axis',(1.,0.,0.));
#8013=DIRECTION('',(0.707106781186547,8.65956056235493E-17,0.707106781186548));
#8014=DIRECTION('center_axis',(0.,0.,1.));
#8015=DIRECTION('ref_axis',(1.,0.,0.));
#8016=DIRECTION('center_axis',(0.,0.,1.));
#8017=DIRECTION('ref_axis',(1.,5.83250561478606E-14,0.));
#8018=DIRECTION('center_axis',(0.,0.,-1.));
#8019=DIRECTION('ref_axis',(1.,5.83250561478606E-14,0.));
#8020=DIRECTION('center_axis',(0.,0.,1.));
#8021=DIRECTION('ref_axis',(1.,0.,0.));
#8022=DIRECTION('center_axis',(-1.60246890531964E-16,-1.,0.));
#8023=DIRECTION('ref_axis',(1.,-1.60246890531964E-16,0.));
#8024=DIRECTION('',(1.,-1.60246890531964E-16,0.));
#8025=DIRECTION('',(0.,0.,1.));
#8026=DIRECTION('',(1.,-1.60246890531964E-16,0.));
#8027=DIRECTION('',(0.,0.,1.));
#8028=DIRECTION('center_axis',(-0.866025403784439,-0.5,0.));
#8029=DIRECTION('ref_axis',(0.5,-0.866025403784439,0.));
#8030=DIRECTION('',(0.5,-0.866025403784439,0.));
#8031=DIRECTION('',(0.,0.,1.));
#8032=DIRECTION('',(0.5,-0.866025403784439,0.));
#8033=DIRECTION('center_axis',(-0.866025403784439,0.5,0.));
#8034=DIRECTION('ref_axis',(-0.5,-0.866025403784439,0.));
#8035=DIRECTION('',(-0.5,-0.866025403784439,0.));
#8036=DIRECTION('',(0.,0.,1.));
#8037=DIRECTION('',(-0.5,-0.866025403784439,0.));
#8038=DIRECTION('center_axis',(1.60246890531964E-16,1.,0.));
#8039=DIRECTION('ref_axis',(-1.,1.60246890531964E-16,0.));
#8040=DIRECTION('',(-1.,1.60246890531964E-16,0.));
#8041=DIRECTION('',(0.,0.,1.));
#8042=DIRECTION('',(-1.,1.60246890531964E-16,0.));
#8043=DIRECTION('center_axis',(0.866025403784439,0.5,0.));
#8044=DIRECTION('ref_axis',(-0.5,0.866025403784439,0.));
#8045=DIRECTION('',(-0.5,0.866025403784439,0.));
#8046=DIRECTION('',(0.,0.,1.));
#8047=DIRECTION('',(-0.5,0.866025403784439,0.));
#8048=DIRECTION('center_axis',(0.866025403784439,-0.5,0.));
#8049=DIRECTION('ref_axis',(0.5,0.866025403784439,0.));
#8050=DIRECTION('',(0.5,0.866025403784439,0.));
#8051=DIRECTION('',(0.5,0.866025403784439,0.));
#8052=DIRECTION('center_axis',(0.,0.,1.));
#8053=DIRECTION('ref_axis',(1.,0.,0.));
#8054=DIRECTION('center_axis',(0.,0.,1.));
#8055=DIRECTION('ref_axis',(1.,0.,0.));
#8056=DIRECTION('center_axis',(0.,0.,1.));
#8057=DIRECTION('ref_axis',(1.,0.,0.));
#8058=DIRECTION('center_axis',(0.,0.,1.));
#8059=DIRECTION('ref_axis',(1.,0.,0.));
#8060=DIRECTION('',(0.,0.,-1.));
#8061=DIRECTION('center_axis',(0.,0.,1.));
#8062=DIRECTION('ref_axis',(1.,0.,0.));
#8063=DIRECTION('center_axis',(0.,0.,1.));
#8064=DIRECTION('ref_axis',(1.,0.,0.));
#8065=DIRECTION('center_axis',(0.,0.,1.));
#8066=DIRECTION('ref_axis',(1.,0.,0.));
#8067=DIRECTION('axis',(0.,0.,1.));
#8068=DIRECTION('refdir',(1.,0.,0.));
#8069=DIRECTION('center_axis',(0.,0.,1.));
#8070=DIRECTION('ref_axis',(1.,0.,0.));
#8071=DIRECTION('',(0.,0.,-1.));
#8072=DIRECTION('center_axis',(0.,0.,-1.));
#8073=DIRECTION('ref_axis',(1.,0.,0.));
#8074=DIRECTION('center_axis',(0.,0.,1.));
#8075=DIRECTION('ref_axis',(1.,0.,0.));
#8076=DIRECTION('',(0.,0.,-1.));
#8077=DIRECTION('center_axis',(0.,0.,1.));
#8078=DIRECTION('ref_axis',(1.,0.,0.));
#8079=DIRECTION('',(0.,0.,-1.));
#8080=DIRECTION('center_axis',(0.,0.,1.));
#8081=DIRECTION('ref_axis',(1.,0.,0.));
#8082=DIRECTION('',(0.,0.,-1.));
#8083=DIRECTION('center_axis',(0.,0.,1.));
#8084=DIRECTION('ref_axis',(1.,0.,0.));
#8085=DIRECTION('',(0.,0.,-1.));
#8086=DIRECTION('center_axis',(0.,0.,1.));
#8087=DIRECTION('ref_axis',(1.,0.,0.));
#8088=DIRECTION('',(0.,0.,-1.));
#8089=DIRECTION('center_axis',(0.,0.,1.));
#8090=DIRECTION('ref_axis',(1.,0.,0.));
#8091=DIRECTION('',(0.,0.,-1.));
#8092=DIRECTION('center_axis',(0.,0.,1.));
#8093=DIRECTION('ref_axis',(1.,0.,0.));
#8094=DIRECTION('',(0.,0.,-1.));
#8095=DIRECTION('center_axis',(0.,0.,1.));
#8096=DIRECTION('ref_axis',(1.,0.,0.));
#8097=DIRECTION('',(0.,0.,-1.));
#8098=DIRECTION('center_axis',(0.,0.,1.));
#8099=DIRECTION('ref_axis',(1.,0.,0.));
#8100=DIRECTION('',(0.,0.,-1.));
#8101=DIRECTION('center_axis',(0.,0.,1.));
#8102=DIRECTION('ref_axis',(1.,0.,0.));
#8103=DIRECTION('',(0.,0.,-1.));
#8104=DIRECTION('center_axis',(0.,0.,1.));
#8105=DIRECTION('ref_axis',(1.,0.,0.));
#8106=DIRECTION('',(0.,0.,-1.));
#8107=DIRECTION('center_axis',(0.,0.,1.));
#8108=DIRECTION('ref_axis',(1.,0.,0.));
#8109=DIRECTION('',(0.,0.,-1.));
#8110=DIRECTION('center_axis',(0.,0.,1.));
#8111=DIRECTION('ref_axis',(1.,0.,0.));
#8112=DIRECTION('',(0.,0.,-1.));
#8113=DIRECTION('center_axis',(0.,0.,1.));
#8114=DIRECTION('ref_axis',(1.,0.,0.));
#8115=DIRECTION('',(0.,0.,-1.));
#8116=DIRECTION('center_axis',(0.,0.,1.));
#8117=DIRECTION('ref_axis',(0.997339946684471,-0.0728905394918792,0.));
#8118=DIRECTION('',(0.,0.,1.));
#8119=DIRECTION('center_axis',(0.,0.,-1.));
#8120=DIRECTION('ref_axis',(1.,1.10476514494527E-13,0.));
#8121=DIRECTION('center_axis',(0.,0.,1.));
#8122=DIRECTION('ref_axis',(1.,1.10476514494527E-13,0.));
#8123=DIRECTION('',(0.,0.,1.));
#8124=DIRECTION('center_axis',(0.,0.,1.));
#8125=DIRECTION('ref_axis',(1.,1.10476514494527E-13,0.));
#8126=DIRECTION('',(0.,0.,1.));
#8127=DIRECTION('center_axis',(0.,0.,1.));
#8128=DIRECTION('ref_axis',(1.,1.10476514494527E-13,0.));
#8129=DIRECTION('',(0.,0.,1.));
#8130=DIRECTION('center_axis',(0.,0.,1.));
#8131=DIRECTION('ref_axis',(1.,1.10476514494527E-13,0.));
#8132=DIRECTION('',(0.,0.,1.));
#8133=DIRECTION('center_axis',(0.,0.,1.));
#8134=DIRECTION('ref_axis',(1.,1.10476514494527E-13,0.));
#8135=DIRECTION('',(0.,0.,1.));
#8136=DIRECTION('center_axis',(0.,0.,1.));
#8137=DIRECTION('ref_axis',(1.,1.10476514494527E-13,0.));
#8138=DIRECTION('',(0.,0.,1.));
#8139=DIRECTION('center_axis',(0.,0.,1.));
#8140=DIRECTION('ref_axis',(1.,1.10476514494527E-13,0.));
#8141=DIRECTION('',(0.,0.,1.));
#8142=DIRECTION('center_axis',(0.,0.,1.));
#8143=DIRECTION('ref_axis',(1.,1.10476514494527E-13,0.));
#8144=DIRECTION('',(0.,0.,1.));
#8145=DIRECTION('center_axis',(0.,0.,1.));
#8146=DIRECTION('ref_axis',(1.,1.10476514494527E-13,0.));
#8147=DIRECTION('',(0.,0.,1.));
#8148=DIRECTION('center_axis',(0.,0.,1.));
#8149=DIRECTION('ref_axis',(1.,1.10476514494527E-13,0.));
#8150=DIRECTION('',(0.,0.,1.));
#8151=DIRECTION('center_axis',(0.,0.,1.));
#8152=DIRECTION('ref_axis',(1.,1.10476514494527E-13,0.));
#8153=DIRECTION('',(0.,0.,1.));
#8154=DIRECTION('center_axis',(0.,0.,1.));
#8155=DIRECTION('ref_axis',(1.,1.10476514494527E-13,0.));
#8156=DIRECTION('',(0.,0.,1.));
#8157=DIRECTION('center_axis',(0.,0.,1.));
#8158=DIRECTION('ref_axis',(1.,1.10476514494527E-13,0.));
#8159=DIRECTION('',(0.,0.,1.));
#8160=DIRECTION('center_axis',(0.,0.,1.));
#8161=DIRECTION('ref_axis',(1.,1.10476514494527E-13,0.));
#8162=DIRECTION('',(0.,0.,1.));
#8163=DIRECTION('center_axis',(0.,0.,-1.));
#8164=DIRECTION('ref_axis',(1.,0.,0.));
#8165=DIRECTION('center_axis',(0.,0.,-1.));
#8166=DIRECTION('ref_axis',(1.,0.,0.));
#8167=DIRECTION('',(0.707106781186547,8.65956056235493E-17,0.707106781186548));
#8168=DIRECTION('center_axis',(0.,0.,1.));
#8169=DIRECTION('ref_axis',(1.,0.,0.));
#8170=DIRECTION('center_axis',(0.,0.,1.));
#8171=DIRECTION('ref_axis',(1.,1.10476514494527E-13,0.));
#8172=DIRECTION('center_axis',(0.,0.,-1.));
#8173=DIRECTION('ref_axis',(1.,1.10476514494527E-13,0.));
#8174=DIRECTION('center_axis',(0.,0.,1.));
#8175=DIRECTION('ref_axis',(1.,0.,0.));
#8176=DIRECTION('center_axis',(-1.92296268638356E-16,-1.,0.));
#8177=DIRECTION('ref_axis',(1.,-1.92296268638356E-16,0.));
#8178=DIRECTION('',(1.,-1.92296268638356E-16,0.));
#8179=DIRECTION('',(0.,0.,1.));
#8180=DIRECTION('',(1.,-1.92296268638356E-16,0.));
#8181=DIRECTION('',(0.,0.,1.));
#8182=DIRECTION('center_axis',(-0.866025403784439,-0.5,0.));
#8183=DIRECTION('ref_axis',(0.5,-0.866025403784439,0.));
#8184=DIRECTION('',(0.5,-0.866025403784439,0.));
#8185=DIRECTION('',(0.,0.,1.));
#8186=DIRECTION('',(0.5,-0.866025403784439,0.));
#8187=DIRECTION('center_axis',(-0.866025403784439,0.5,0.));
#8188=DIRECTION('ref_axis',(-0.5,-0.866025403784438,0.));
#8189=DIRECTION('',(-0.5,-0.866025403784438,0.));
#8190=DIRECTION('',(0.,0.,1.));
#8191=DIRECTION('',(-0.5,-0.866025403784439,0.));
#8192=DIRECTION('center_axis',(1.92296268638356E-16,1.,0.));
#8193=DIRECTION('ref_axis',(-1.,1.92296268638356E-16,0.));
#8194=DIRECTION('',(-1.,1.92296268638356E-16,0.));
#8195=DIRECTION('',(0.,0.,1.));
#8196=DIRECTION('',(-1.,1.92296268638356E-16,0.));
#8197=DIRECTION('center_axis',(0.866025403784439,0.5,0.));
#8198=DIRECTION('ref_axis',(-0.5,0.866025403784439,0.));
#8199=DIRECTION('',(-0.5,0.866025403784439,0.));
#8200=DIRECTION('',(0.,0.,1.));
#8201=DIRECTION('',(-0.5,0.866025403784439,0.));
#8202=DIRECTION('center_axis',(0.866025403784439,-0.5,0.));
#8203=DIRECTION('ref_axis',(0.5,0.866025403784439,0.));
#8204=DIRECTION('',(0.5,0.866025403784439,0.));
#8205=DIRECTION('',(0.5,0.866025403784439,0.));
#8206=DIRECTION('center_axis',(0.,0.,1.));
#8207=DIRECTION('ref_axis',(1.,0.,0.));
#8208=DIRECTION('center_axis',(0.,0.,1.));
#8209=DIRECTION('ref_axis',(1.,0.,0.));
#8210=DIRECTION('center_axis',(0.,0.,1.));
#8211=DIRECTION('ref_axis',(1.,0.,0.));
#8212=DIRECTION('center_axis',(0.,0.,1.));
#8213=DIRECTION('ref_axis',(1.,0.,0.));
#8214=DIRECTION('',(0.,0.,-1.));
#8215=DIRECTION('center_axis',(0.,0.,1.));
#8216=DIRECTION('ref_axis',(1.,0.,0.));
#8217=DIRECTION('center_axis',(0.,0.,1.));
#8218=DIRECTION('ref_axis',(1.,0.,0.));
#8219=DIRECTION('center_axis',(0.,0.,1.));
#8220=DIRECTION('ref_axis',(1.,0.,0.));
#8221=DIRECTION('axis',(0.,0.,1.));
#8222=DIRECTION('refdir',(1.,0.,0.));
#8223=DIRECTION('center_axis',(0.,0.,1.));
#8224=DIRECTION('ref_axis',(1.,0.,0.));
#8225=DIRECTION('center_axis',(0.,0.,-1.));
#8226=DIRECTION('ref_axis',(1.,0.,0.));
#8227=DIRECTION('',(0.,0.,-1.));
#8228=DIRECTION('center_axis',(0.,0.,-1.));
#8229=DIRECTION('ref_axis',(1.,0.,0.));
#8230=DIRECTION('center_axis',(0.,0.,1.));
#8231=DIRECTION('ref_axis',(1.,0.,0.));
#8232=DIRECTION('center_axis',(0.,0.,1.));
#8233=DIRECTION('ref_axis',(1.,0.,0.));
#8234=DIRECTION('',(0.,0.,-1.));
#8235=DIRECTION('center_axis',(0.,0.,1.));
#8236=DIRECTION('ref_axis',(1.,0.,0.));
#8237=DIRECTION('center_axis',(0.,0.,1.));
#8238=DIRECTION('ref_axis',(1.,0.,0.));
#8239=DIRECTION('center_axis',(0.,0.,1.));
#8240=DIRECTION('ref_axis',(1.,0.,0.));
#8241=DIRECTION('axis',(0.,0.,1.));
#8242=DIRECTION('refdir',(1.,0.,0.));
#8243=DIRECTION('center_axis',(0.,0.,-1.));
#8244=DIRECTION('ref_axis',(-0.346824478021586,0.937930051467088,0.));
#8245=DIRECTION('',(0.,0.,-1.));
#8246=DIRECTION('center_axis',(0.,0.,-1.));
#8247=DIRECTION('ref_axis',(1.,0.,0.));
#8248=DIRECTION('center_axis',(0.,0.,-1.));
#8249=DIRECTION('ref_axis',(1.,0.,0.));
#8250=DIRECTION('',(0.,0.,-1.));
#8251=DIRECTION('center_axis',(0.,0.,-1.));
#8252=DIRECTION('ref_axis',(1.,0.,0.));
#8253=DIRECTION('',(0.,0.,-1.));
#8254=DIRECTION('center_axis',(0.,0.,-1.));
#8255=DIRECTION('ref_axis',(1.,0.,0.));
#8256=DIRECTION('',(0.,0.,-1.));
#8257=DIRECTION('center_axis',(0.,0.,-1.));
#8258=DIRECTION('ref_axis',(0.937996590358642,-0.346644481386278,0.));
#8259=DIRECTION('',(0.,0.,-1.));
#8260=DIRECTION('center_axis',(0.,0.,-1.));
#8261=DIRECTION('ref_axis',(1.,0.,0.));
#8262=DIRECTION('center_axis',(0.,0.,-1.));
#8263=DIRECTION('ref_axis',(0.7932173491397,0.608938615152452,0.));
#8264=DIRECTION('',(1.22464679914735E-16,-9.27389451825078E-31,-1.));
#8265=DIRECTION('center_axis',(0.,0.,1.));
#8266=DIRECTION('ref_axis',(1.,-7.45024487577726E-15,0.));
#8267=DIRECTION('center_axis',(0.,0.,-1.));
#8268=DIRECTION('ref_axis',(1.,-7.45024487577726E-15,0.));
#8269=DIRECTION('',(1.22464679914735E-16,-9.27389451825078E-31,-1.));
#8270=DIRECTION('center_axis',(0.,0.,-1.));
#8271=DIRECTION('ref_axis',(1.,-7.45024487577726E-15,0.));
#8272=DIRECTION('',(1.22464679914735E-16,-9.27389451825078E-31,-1.));
#8273=DIRECTION('center_axis',(0.,0.,-1.));
#8274=DIRECTION('ref_axis',(1.,-7.45024487577726E-15,0.));
#8275=DIRECTION('',(1.22464679914735E-16,-9.27389451825078E-31,-1.));
#8276=DIRECTION('center_axis',(0.,0.,-1.));
#8277=DIRECTION('ref_axis',(-0.609064819364946,-0.793120448489348,0.));
#8278=DIRECTION('',(1.22464679914735E-16,-9.27389451825078E-31,-1.));
#8279=DIRECTION('center_axis',(0.,0.,-1.));
#8280=DIRECTION('ref_axis',(1.,-7.45024487577726E-15,0.));
#8281=DIRECTION('center_axis',(0.,0.,-1.));
#8282=DIRECTION('ref_axis',(1.,-7.45024487577726E-15,0.));
#8283=DIRECTION('center_axis',(0.,0.,1.));
#8284=DIRECTION('ref_axis',(1.,0.,0.));
#8285=DIRECTION('',(0.5,0.866025403784439,0.));
#8286=DIRECTION('',(-0.5,0.866025403784439,0.));
#8287=DIRECTION('',(-1.,1.92296268638356E-16,0.));
#8288=DIRECTION('',(-0.5,-0.866025403784439,0.));
#8289=DIRECTION('',(0.5,-0.866025403784439,0.));
#8290=DIRECTION('',(1.,-1.92296268638356E-16,0.));
#8291=DIRECTION('center_axis',(0.,0.,-1.));
#8292=DIRECTION('ref_axis',(1.,0.,0.));
#8293=DIRECTION('center_axis',(-1.92296268638356E-16,-1.,0.));
#8294=DIRECTION('ref_axis',(1.,-1.92296268638356E-16,0.));
#8295=DIRECTION('',(1.,-1.92296268638356E-16,0.));
#8296=DIRECTION('',(0.,0.,1.));
#8297=DIRECTION('',(0.,0.,1.));
#8298=DIRECTION('center_axis',(-0.866025403784439,-0.5,0.));
#8299=DIRECTION('ref_axis',(0.5,-0.866025403784439,0.));
#8300=DIRECTION('',(0.5,-0.866025403784439,0.));
#8301=DIRECTION('',(0.,0.,1.));
#8302=DIRECTION('center_axis',(-0.866025403784439,0.5,0.));
#8303=DIRECTION('ref_axis',(-0.5,-0.866025403784438,0.));
#8304=DIRECTION('',(-0.5,-0.866025403784439,0.));
#8305=DIRECTION('',(0.,0.,1.));
#8306=DIRECTION('center_axis',(1.92296268638356E-16,1.,0.));
#8307=DIRECTION('ref_axis',(-1.,1.92296268638356E-16,0.));
#8308=DIRECTION('',(-1.,1.92296268638356E-16,0.));
#8309=DIRECTION('',(0.,0.,1.));
#8310=DIRECTION('center_axis',(0.866025403784439,0.5,0.));
#8311=DIRECTION('ref_axis',(-0.5,0.866025403784439,0.));
#8312=DIRECTION('',(-0.5,0.866025403784439,0.));
#8313=DIRECTION('',(0.,0.,1.));
#8314=DIRECTION('center_axis',(0.866025403784439,-0.5,0.));
#8315=DIRECTION('ref_axis',(0.5,0.866025403784439,0.));
#8316=DIRECTION('',(0.5,0.866025403784439,0.));
#8317=DIRECTION('center_axis',(0.,0.,1.));
#8318=DIRECTION('ref_axis',(1.,0.,0.));
#8319=DIRECTION('',(0.,0.,1.));
#8320=DIRECTION('',(1.,0.,0.));
#8321=DIRECTION('',(0.,0.,1.));
#8322=DIRECTION('',(1.,0.,0.));
#8323=DIRECTION('',(0.,0.,1.));
#8324=DIRECTION('',(1.,0.,0.));
#8325=DIRECTION('',(0.,0.,1.));
#8326=DIRECTION('',(1.,0.,0.));
#8327=DIRECTION('',(0.,0.,1.));
#8328=DIRECTION('',(1.,0.,0.));
#8329=DIRECTION('',(0.,0.,1.));
#8330=DIRECTION('',(1.,0.,0.));
#8331=DIRECTION('',(0.,0.,1.));
#8332=DIRECTION('',(-2.22044604925031E-16,-1.,0.));
#8333=DIRECTION('',(0.,-1.22464679914735E-16,-1.));
#8334=DIRECTION('',(1.,0.,0.));
#8335=DIRECTION('',(0.,0.,1.));
#8336=DIRECTION('',(1.,0.,0.));
#8337=DIRECTION('',(0.,0.,1.));
#8338=DIRECTION('',(1.,0.,0.));
#8339=DIRECTION('',(0.,0.,1.));
#8340=DIRECTION('',(1.,0.,0.));
#8341=DIRECTION('',(0.,0.,1.));
#8342=DIRECTION('',(-2.22044604925031E-16,-1.,0.));
#8343=DIRECTION('',(0.,0.,1.));
#8344=DIRECTION('',(-2.22044604925031E-16,-1.,0.));
#8345=DIRECTION('',(0.,0.,1.));
#8346=DIRECTION('',(-2.22044604925031E-16,-1.,0.));
#8347=DIRECTION('',(0.,-1.22464679914735E-16,-1.));
#8348=DIRECTION('',(1.,0.,0.));
#8349=DIRECTION('',(0.,0.,1.));
#8350=DIRECTION('',(1.,0.,0.));
#8351=DIRECTION('',(0.,0.,1.));
#8352=DIRECTION('',(1.,0.,0.));
#8353=CARTESIAN_POINT('',(0.,0.,0.));
#8354=CARTESIAN_POINT('',(0.,0.,0.));
#8355=CARTESIAN_POINT('Origin',(15.,10.,4.));
#8356=CARTESIAN_POINT('',(13.3328088490546,10.0013492358765,0.571480363390205));
#8357=CARTESIAN_POINT('',(13.3364070293386,10.0006645492999,0.378519636609792));
#8358=CARTESIAN_POINT('',(13.334,10.,4.));
#8359=CARTESIAN_POINT('',(16.6117095221421,9.57816067485776,0.));
#8360=CARTESIAN_POINT('Ctrl Pts',(13.3364070293386,10.0006645492999,0.378519636609792));
#8361=CARTESIAN_POINT('Ctrl Pts',(13.3354289147321,10.2261439494212,0.363487571935548));
#8362=CARTESIAN_POINT('Ctrl Pts',(13.3780964617564,10.4512892386983,0.348455507261304));
#8363=CARTESIAN_POINT('Ctrl Pts',(13.4661891862405,10.6570298059976,0.33342344258706));
#8364=CARTESIAN_POINT('Ctrl Pts',(13.6832967870101,11.1640846304335,0.29637639341072));
#8365=CARTESIAN_POINT('Ctrl Pts',(14.1763138565653,11.5532764803646,0.259329344234379));
#8366=CARTESIAN_POINT('Ctrl Pts',(14.7201523395477,11.6454139726504,0.222282295058039));
#8367=CARTESIAN_POINT('Ctrl Pts',(15.2639908225302,11.7375514649362,0.185235245881699));
#8368=CARTESIAN_POINT('Ctrl Pts',(15.8586507189399,11.5326345995767,0.14818819670536));
#8369=CARTESIAN_POINT('Ctrl Pts',(16.230649324425,11.1267737685767,0.11114114752902));
#8370=CARTESIAN_POINT('Ctrl Pts',(16.6026479299101,10.7209129375768,0.074094098352681));
#8371=CARTESIAN_POINT('Ctrl Pts',(16.7519852444706,10.1141081409362,0.0370470491763412));
#8372=CARTESIAN_POINT('Ctrl Pts',(16.6117095221421,9.5781606748578,2.42861286636753E-15));
#8373=CARTESIAN_POINT('',(14.324922814325,8.47690223774665,0.));
#8374=CARTESIAN_POINT('Origin',(15.,10.,0.));
#8375=CARTESIAN_POINT('Ctrl Pts',(14.3235905172155,8.47417638326182,1.73472347597681E-17));
#8376=CARTESIAN_POINT('Ctrl Pts',(14.8183179067709,8.25559293309757,0.0363261751465299));
#8377=CARTESIAN_POINT('Ctrl Pts',(15.4299365639682,8.29934549446852,0.0726523502930599));
#8378=CARTESIAN_POINT('Ctrl Pts',(15.8878245545432,8.58718953131908,0.10897852543959));
#8379=CARTESIAN_POINT('Ctrl Pts',(16.354799093857,8.88074568319316,0.14602557461593));
#8380=CARTESIAN_POINT('Ctrl Pts',(16.6618810168406,9.42817717104187,0.18307262379227));
#8381=CARTESIAN_POINT('Ctrl Pts',(16.6686053025862,9.97953156441245,0.22011967296861));
#8382=CARTESIAN_POINT('Ctrl Pts',(16.6753295883318,10.530885957783,0.257166722144951));
#8383=CARTESIAN_POINT('Ctrl Pts',(16.3816962368394,11.0861632566755,0.294213771321291));
#8384=CARTESIAN_POINT('Ctrl Pts',(15.9220537145076,11.3909183482768,0.331260820497631));
#8385=CARTESIAN_POINT('Ctrl Pts',(15.4624111921758,11.6956734398782,0.368307869673971));
#8386=CARTESIAN_POINT('Ctrl Pts',(14.8367594990047,11.7499063241884,0.405354918850311));
#8387=CARTESIAN_POINT('Ctrl Pts',(14.3314685943663,11.5289531757505,0.442401968026651));
#8388=CARTESIAN_POINT('Ctrl Pts',(13.8261776897279,11.3080000273125,0.479449017202991));
#8389=CARTESIAN_POINT('Ctrl Pts',(13.4412475736223,10.8118608461263,0.516496066379331));
#8390=CARTESIAN_POINT('Ctrl Pts',(13.3528420328787,10.2675275034982,0.55354311555567));
#8391=CARTESIAN_POINT('Ctrl Pts',(13.338574121043,10.1796766733746,0.559522198167182));
#8392=CARTESIAN_POINT('Ctrl Pts',(13.3320298587031,10.0905705179199,0.565501280778694));
#8393=CARTESIAN_POINT('Ctrl Pts',(13.3328088490546,10.0013492358765,0.571480363390205));
#8394=CARTESIAN_POINT('Origin',(15.,10.,4.));
#8395=CARTESIAN_POINT('',(13.3366506987084,10.0003647761852,1.27148036339021));
#8396=CARTESIAN_POINT('',(13.3350093517191,9.9985620319516,1.07851963660979));
#8397=CARTESIAN_POINT('',(13.334,10.,4.));
#8398=CARTESIAN_POINT('Ctrl Pts',(13.3350093517191,9.9985620319516,1.07851963660979));
#8399=CARTESIAN_POINT('Ctrl Pts',(13.3382277662221,10.3890985886774,1.05243653366026));
#8400=CARTESIAN_POINT('Ctrl Pts',(13.4753923609414,10.7816700702397,1.02635343071072));
#8401=CARTESIAN_POINT('Ctrl Pts',(13.7262226055549,11.0780443718138,1.00027032776118));
#8402=CARTESIAN_POINT('Ctrl Pts',(14.0824885155229,11.498998632749,0.963223278584839));
#8403=CARTESIAN_POINT('Ctrl Pts',(14.6680617736869,11.7258861702055,0.9261762294085));
#8404=CARTESIAN_POINT('Ctrl Pts',(15.214946994521,11.6548455259047,0.88912918023216));
#8405=CARTESIAN_POINT('Ctrl Pts',(15.761832215355,11.5838048816039,0.85208213105582));
#8406=CARTESIAN_POINT('Ctrl Pts',(16.2700293988592,11.2148360555457,0.81503508187948));
#8407=CARTESIAN_POINT('Ctrl Pts',(16.5069275188232,10.7168466062646,0.77798803270314));
#8408=CARTESIAN_POINT('Ctrl Pts',(16.7438256387873,10.2188571569834,0.7409409835268));
#8409=CARTESIAN_POINT('Ctrl Pts',(16.7094246952114,9.59184708447927,0.703893934350459));
#8410=CARTESIAN_POINT('Ctrl Pts',(16.4195065689417,9.12271321406216,0.666846885174119));
#8411=CARTESIAN_POINT('Ctrl Pts',(16.1295884426719,8.65357934364505,0.62979983599778));
#8412=CARTESIAN_POINT('Ctrl Pts',(15.5841531337084,8.34232167531498,0.59275278682144));
#8413=CARTESIAN_POINT('Ctrl Pts',(15.032763395353,8.33153873726589,0.5557057376451));
#8414=CARTESIAN_POINT('Ctrl Pts',(14.4813736569975,8.32075579921679,0.518658688468759));
#8415=CARTESIAN_POINT('Ctrl Pts',(13.9240294892501,8.61044759144868,0.481611639292419));
#8416=CARTESIAN_POINT('Ctrl Pts',(13.6159564713684,9.06775238703494,0.444564590116079));
#8417=CARTESIAN_POINT('Ctrl Pts',(13.4328859471306,9.33950299096684,0.422549605613983));
#8418=CARTESIAN_POINT('Ctrl Pts',(13.337839512392,9.67044208107719,0.400534621111888));
#8419=CARTESIAN_POINT('Ctrl Pts',(13.3364070293386,10.0006645492999,0.378519636609792));
#8420=CARTESIAN_POINT('Ctrl Pts',(13.3328088490546,10.0013492358765,0.571480363390205));
#8421=CARTESIAN_POINT('Ctrl Pts',(13.3368565680386,9.5377457054525,0.602548329955034));
#8422=CARTESIAN_POINT('Ctrl Pts',(13.5386288253055,9.07103380876728,0.633616296519862));
#8423=CARTESIAN_POINT('Ctrl Pts',(13.8819529042008,8.76117501449623,0.664684263084691));
#8424=CARTESIAN_POINT('Ctrl Pts',(14.2913502816478,8.39168337219233,0.70173131226103));
#8425=CARTESIAN_POINT('Ctrl Pts',(14.9020260019234,8.24522759165455,0.73877836143737));
#8426=CARTESIAN_POINT('Ctrl Pts',(15.4344829009358,8.38881597583482,0.77582541061371));
#8427=CARTESIAN_POINT('Ctrl Pts',(15.9669397999483,8.53240436001509,0.81287245979005));
#8428=CARTESIAN_POINT('Ctrl Pts',(16.4211778776976,8.96603690891341,0.84991950896639));
#8429=CARTESIAN_POINT('Ctrl Pts',(16.589302871581,9.49125972577423,0.88696655814273));
#8430=CARTESIAN_POINT('Ctrl Pts',(16.7574278654643,10.0164825426351,0.92401360731907));
#8431=CARTESIAN_POINT('Ctrl Pts',(16.6394397754816,10.6332956274584,0.961060656495409));
#8432=CARTESIAN_POINT('Ctrl Pts',(16.2893386307264,11.0593900732881,0.998107705671749));
#8433=CARTESIAN_POINT('Ctrl Pts',(15.9392374859711,11.4854845191178,1.03515475484809));
#8434=CARTESIAN_POINT('Ctrl Pts',(15.3570232864432,11.7208603259538,1.07220180402443));
#8435=CARTESIAN_POINT('Ctrl Pts',(14.8091643682469,11.6577936066139,1.10924885320077));
#8436=CARTESIAN_POINT('Ctrl Pts',(14.2613054500506,11.594726887274,1.14629590237711));
#8437=CARTESIAN_POINT('Ctrl Pts',(13.7478018131859,11.2332176417582,1.18334295155345));
#8438=CARTESIAN_POINT('Ctrl Pts',(13.5036737118494,10.7387199750775,1.22039000072979));
#8439=CARTESIAN_POINT('Ctrl Pts',(13.3914507097464,10.5114048385405,1.2374201216166));
#8440=CARTESIAN_POINT('Ctrl Pts',(13.3361505226053,10.255987390206,1.2544502425034));
#8441=CARTESIAN_POINT('Ctrl Pts',(13.3366506987084,10.0003647761852,1.27148036339021));
#8442=CARTESIAN_POINT('Origin',(15.,10.,4.));
#8443=CARTESIAN_POINT('',(13.3341440524774,9.99847620463016,1.97148036339021));
#8444=CARTESIAN_POINT('',(13.3312583494731,10.0000242625446,1.77851963660979));
#8445=CARTESIAN_POINT('',(13.334,10.,4.));
#8446=CARTESIAN_POINT('Ctrl Pts',(13.3312588297318,10.0000242582945,1.77851963660979));
#8447=CARTESIAN_POINT('Ctrl Pts',(13.3311401928165,10.5527978235745,1.74138549538496));
#8448=CARTESIAN_POINT('Ctrl Pts',(13.633172617078,11.1054588469535,1.70425135416013));
#8449=CARTESIAN_POINT('Ctrl Pts',(14.0982990092452,11.4041487296504,1.6671172129353));
#8450=CARTESIAN_POINT('Ctrl Pts',(14.562334523612,11.7021380841302,1.63007016375896));
#8451=CARTESIAN_POINT('Ctrl Pts',(15.1886983700061,11.7473461999417,1.59302311458262));
#8452=CARTESIAN_POINT('Ctrl Pts',(15.6907163851895,11.5190818474979,1.55597606540628));
#8453=CARTESIAN_POINT('Ctrl Pts',(16.1927344003729,11.2908174950541,1.51892901622994));
#8454=CARTESIAN_POINT('Ctrl Pts',(16.5704065843456,10.789080674355,1.4818819670536));
#8455=CARTESIAN_POINT('Ctrl Pts',(16.650879481241,10.2435071243058,1.44483491787726));
#8456=CARTESIAN_POINT('Ctrl Pts',(16.7313523781363,9.69793357425666,1.40778786870092));
#8457=CARTESIAN_POINT('Ctrl Pts',(16.5146259879544,9.10852329485745,1.37074081952458));
#8458=CARTESIAN_POINT('Ctrl Pts',(16.0998923987615,8.74503633532444,1.33369377034824));
#8459=CARTESIAN_POINT('Ctrl Pts',(15.6851588095687,8.38154937579143,1.2966467211719));
#8460=CARTESIAN_POINT('Ctrl Pts',(15.072418021365,8.24398573612463,1.25959967199556));
#8461=CARTESIAN_POINT('Ctrl Pts',(14.5421080170767,8.39530825722336,1.22255262281922));
#8462=CARTESIAN_POINT('Ctrl Pts',(14.0117980127884,8.5466307783221,1.18550557364288));
#8463=CARTESIAN_POINT('Ctrl Pts',(13.5639187924156,8.98683946018636,1.14845852446654));
#8464=CARTESIAN_POINT('Ctrl Pts',(13.4034584631152,9.51445429332549,1.1114114752902));
#8465=CARTESIAN_POINT('Ctrl Pts',(13.3559707829599,9.67060008057741,1.1004475290634));
#8466=CARTESIAN_POINT('Ctrl Pts',(13.3336565018065,9.83440127945886,1.0894835828366));
#8467=CARTESIAN_POINT('Ctrl Pts',(13.3350093517191,9.9985620319516,1.07851963660979));
#8468=CARTESIAN_POINT('Ctrl Pts',(13.3366506987084,10.0003647761852,1.27148036339021));
#8469=CARTESIAN_POINT('Ctrl Pts',(13.3372385975997,9.69991009544355,1.29149729167974));
#8470=CARTESIAN_POINT('Ctrl Pts',(13.4149162099074,9.39917197274857,1.31151421996928));
#8471=CARTESIAN_POINT('Ctrl Pts',(13.5678608709571,9.14345047930851,1.33153114825881));
#8472=CARTESIAN_POINT('Ctrl Pts',(13.8509286972094,8.67016473806549,1.36857819743515));
#8473=CARTESIAN_POINT('Ctrl Pts',(14.3918169155223,8.3510793434248,1.40562524661149));
#8474=CARTESIAN_POINT('Ctrl Pts',(14.9429716248518,8.3322329656282,1.44267229578783));
#8475=CARTESIAN_POINT('Ctrl Pts',(15.4941263341813,8.31338658783161,1.47971934496417));
#8476=CARTESIAN_POINT('Ctrl Pts',(16.0555475345274,8.59477922687911,1.51676639414051));
#8477=CARTESIAN_POINT('Ctrl Pts',(16.3702838693714,9.04762324449391,1.55381344331685));
#8478=CARTESIAN_POINT('Ctrl Pts',(16.6850202042153,9.50046726210872,1.59086049249319));
#8479=CARTESIAN_POINT('Ctrl Pts',(16.7530716735571,10.1247626582908,1.62790754166953));
#8480=CARTESIAN_POINT('Ctrl Pts',(16.543292450279,10.6347816628546,1.66495459084587));
#8481=CARTESIAN_POINT('Ctrl Pts',(16.3335132270009,11.1448006674184,1.70200164002221));
#8482=CARTESIAN_POINT('Ctrl Pts',(15.8459033111031,11.5405432803638,1.73904868919855));
#8483=CARTESIAN_POINT('Ctrl Pts',(15.3036321297176,11.6408859866488,1.77609573837489));
#8484=CARTESIAN_POINT('Ctrl Pts',(14.7613609483321,11.7412286929337,1.81314278755123));
#8485=CARTESIAN_POINT('Ctrl Pts',(14.1644285014591,11.5461714925582,1.85018983672757));
#8486=CARTESIAN_POINT('Ctrl Pts',(13.7860389659804,11.1449881814256,1.88723688590391));
#8487=CARTESIAN_POINT('Ctrl Pts',(13.4992248469807,10.8408966906439,1.91531804506601));
#8488=CARTESIAN_POINT('Ctrl Pts',(13.3379731090858,10.4183768092574,1.94339920422811));
#8489=CARTESIAN_POINT('Ctrl Pts',(13.3341440524774,9.99847620463016,1.97148036339021));
#8490=CARTESIAN_POINT('Origin',(15.,10.,4.));
#8491=CARTESIAN_POINT('',(13.3314908561079,10.0005637456851,2.67148036339021));
#8492=CARTESIAN_POINT('',(13.3350798111394,10.0014222545761,2.4785196366098));
#8493=CARTESIAN_POINT('',(13.334,10.,4.));
#8494=CARTESIAN_POINT('Ctrl Pts',(13.3350798111394,10.0014222545761,2.4785196366098));
#8495=CARTESIAN_POINT('Ctrl Pts',(13.3337246262576,10.1682098032958,2.46738150628601));
#8496=CARTESIAN_POINT('Ctrl Pts',(13.356768377288,10.3346314141306,2.45624337596222));
#8497=CARTESIAN_POINT('Ctrl Pts',(13.4057541973467,10.4930302810831,2.44510524563844));
#8498=CARTESIAN_POINT('Ctrl Pts',(13.568688193619,11.0198880608789,2.4080581964621));
#8499=CARTESIAN_POINT('Ctrl Pts',(14.018625736829,11.4579882343367,2.37101114728576));
#8500=CARTESIAN_POINT('Ctrl Pts',(14.5496393059462,11.6068210159811,2.33396409810942));
#8501=CARTESIAN_POINT('Ctrl Pts',(15.0806528750634,11.7556537976255,2.29691704893308));
#8502=CARTESIAN_POINT('Ctrl Pts',(15.6927424700877,11.6152191874565,2.25986999975674));
#8503=CARTESIAN_POINT('Ctrl Pts',(16.1057667866446,11.2497913234872,2.2228229505804));
#8504=CARTESIAN_POINT('Ctrl Pts',(16.5187911032016,10.884363459518,2.18577590140406));
#8505=CARTESIAN_POINT('Ctrl Pts',(16.7327501412913,10.2939423417484,2.14872885222772));
#8506=CARTESIAN_POINT('Ctrl Pts',(16.6497190718447,9.74875205788567,2.11168180305138));
#8507=CARTESIAN_POINT('Ctrl Pts',(16.5666880023982,9.20356177402293,2.07463475387504));
#8508=CARTESIAN_POINT('Ctrl Pts',(16.1866668254153,8.70360232406701,2.0375877046987));
#8509=CARTESIAN_POINT('Ctrl Pts',(15.6835837346665,8.47769523896532,2.00054065552236));
#8510=CARTESIAN_POINT('Ctrl Pts',(15.1805006439177,8.25178815386362,1.96349360634602));
#8511=CARTESIAN_POINT('Ctrl Pts',(14.5543556394029,8.29993343361615,1.92644655716968));
#8512=CARTESIAN_POINT('Ctrl Pts',(14.0917228863641,8.60009598607672,1.88939950799334));
#8513=CARTESIAN_POINT('Ctrl Pts',(13.6301777134446,8.89955290145806,1.85243955086549));
#8514=CARTESIAN_POINT('Ctrl Pts',(13.3313769101603,9.44984357280461,1.81547959373764));
#8515=CARTESIAN_POINT('Ctrl Pts',(13.3312588297318,10.0000242582945,1.77851963660979));
#8516=CARTESIAN_POINT('Ctrl Pts',(13.3341440524774,9.99847620463016,1.97148036339021));
#8517=CARTESIAN_POINT('Ctrl Pts',(13.3329214925321,9.86440828327876,1.98044625340445));
#8518=CARTESIAN_POINT('Ctrl Pts',(13.3477470486685,9.73060737845345,1.98941214341869));
#8519=CARTESIAN_POINT('Ctrl Pts',(13.379657735774,9.60101344779502,1.99837803343293));
#8520=CARTESIAN_POINT('Ctrl Pts',(13.5115126651307,9.06553144718687,2.03542508260927));
#8521=CARTESIAN_POINT('Ctrl Pts',(13.9350691479286,8.6018768678603,2.07247213178561));
#8522=CARTESIAN_POINT('Ctrl Pts',(14.4564737537651,8.42225523761979,2.10951918096195));
#8523=CARTESIAN_POINT('Ctrl Pts',(14.9778783596017,8.24263360737928,2.14656623013829));
#8524=CARTESIAN_POINT('Ctrl Pts',(15.5971310884769,8.34704492622482,2.18361327931463));
#8525=CARTESIAN_POINT('Ctrl Pts',(16.030812208256,8.68770220147219,2.22066032849097));
#8526=CARTESIAN_POINT('Ctrl Pts',(16.4644933280352,9.02835947671956,2.25770737766731));
#8527=CARTESIAN_POINT('Ctrl Pts',(16.7126028387182,9.60526270836876,2.29475442684365));
#8528=CARTESIAN_POINT('Ctrl Pts',(16.6615859215914,10.1543746894207,2.33180147601999));
#8529=CARTESIAN_POINT('Ctrl Pts',(16.6105690044646,10.7034866704727,2.36884852519633));
#8530=CARTESIAN_POINT('Ctrl Pts',(16.2604256595279,11.2248074009274,2.40589557437267));
#8531=CARTESIAN_POINT('Ctrl Pts',(15.7714095743024,11.4797386889282,2.44294262354901));
#8532=CARTESIAN_POINT('Ctrl Pts',(15.282393489077,11.7346699769289,2.47998967272535));
#8533=CARTESIAN_POINT('Ctrl Pts',(14.6545046635628,11.7232118224755,2.51703672190169));
#8534=CARTESIAN_POINT('Ctrl Pts',(14.1751154010763,11.4506083958144,2.55408377107803));
#8535=CARTESIAN_POINT('Ctrl Pts',(13.6957261385897,11.1780049691532,2.59113082025437));
#8536=CARTESIAN_POINT('Ctrl Pts',(13.3648364391308,10.6442562702842,2.62817786943071));
#8537=CARTESIAN_POINT('Ctrl Pts',(13.3338879771839,10.0936485278662,2.66522491860705));
#8538=CARTESIAN_POINT('Ctrl Pts',(13.3321460805134,10.0626582384328,2.6673100668681));
#8539=CARTESIAN_POINT('Ctrl Pts',(13.3313543571281,10.0316145418291,2.66939521512915));
#8540=CARTESIAN_POINT('Ctrl Pts',(13.3314908561079,10.0005637456851,2.67148036339021));
#8541=CARTESIAN_POINT('Origin',(15.,10.,4.));
#8542=CARTESIAN_POINT('',(13.3358101889457,10.0011694310247,3.37148036339021));
#8543=CARTESIAN_POINT('',(13.3362901345243,9.99914721744613,3.1785196366098));
#8544=CARTESIAN_POINT('',(13.334,10.,4.));
#8545=CARTESIAN_POINT('Ctrl Pts',(13.3362901345243,9.99914721744613,3.1785196366098));
#8546=CARTESIAN_POINT('Ctrl Pts',(13.3378337351605,10.3320266569125,3.15633046801072));
#8547=CARTESIAN_POINT('Ctrl Pts',(13.4345606138998,10.6657320713228,3.13414129941164));
#8548=CARTESIAN_POINT('Ctrl Pts',(13.6203848363125,10.9388080400732,3.11195213081256));
#8549=CARTESIAN_POINT('Ctrl Pts',(13.9306370692944,11.394735840973,3.07490508163622));
#8550=CARTESIAN_POINT('Ctrl Pts',(14.489254042355,11.6816550509133,3.03785803245987));
#8551=CARTESIAN_POINT('Ctrl Pts',(15.0405678095774,11.6682484193642,3.00081098328353));
#8552=CARTESIAN_POINT('Ctrl Pts',(15.5918815767999,11.6548417878151,2.96376393410719));
#8553=CARTESIAN_POINT('Ctrl Pts',(16.1358921381843,11.3411093147767,2.92671688493086));
#8554=CARTESIAN_POINT('Ctrl Pts',(16.4236166138013,10.8706401511932,2.88966983575452));
#8555=CARTESIAN_POINT('Ctrl Pts',(16.7113410894183,10.4001709876096,2.85262278657818));
#8556=CARTESIAN_POINT('Ctrl Pts',(16.7427794792678,9.77296513348092,2.81557573740183));
#8557=CARTESIAN_POINT('Ctrl Pts',(16.5035430536575,9.27608230995051,2.7785286882255));
#8558=CARTESIAN_POINT('Ctrl Pts',(16.2643066280471,8.7791994864201,2.74148163904916));
#8559=CARTESIAN_POINT('Ctrl Pts',(15.7543953869767,8.41263969348797,2.70443458987282));
#8560=CARTESIAN_POINT('Ctrl Pts',(15.207185625858,8.34417010176588,2.66738754069648));
#8561=CARTESIAN_POINT('Ctrl Pts',(14.6599758647393,8.27570051004378,2.63034049152014));
#8562=CARTESIAN_POINT('Ctrl Pts',(14.0754675835721,8.50532111953174,2.59329344234379));
#8563=CARTESIAN_POINT('Ctrl Pts',(13.7211786676559,8.92793911734263,2.55624639316745));
#8564=CARTESIAN_POINT('Ctrl Pts',(13.4734060925949,9.22349775573222,2.5303374743149));
#8565=CARTESIAN_POINT('Ctrl Pts',(13.3382321692202,9.61345004202563,2.50442855546235));
#8566=CARTESIAN_POINT('Ctrl Pts',(13.3350798111394,10.0014222545761,2.4785196366098));
#8567=CARTESIAN_POINT('Ctrl Pts',(13.3314908561079,10.0005637456851,2.67148036339021));
#8568=CARTESIAN_POINT('Ctrl Pts',(13.3337795489059,9.47993177029892,2.70644226430549));
#8569=CARTESIAN_POINT('Ctrl Pts',(13.5970248044157,8.95730385981114,2.74140416522078));
#8570=CARTESIAN_POINT('Ctrl Pts',(14.017753627907,8.65096650012722,2.77636606613607));
#8571=CARTESIAN_POINT('Ctrl Pts',(14.4635749650119,8.3263590007736,2.81341311531241));
#8572=CARTESIAN_POINT('Ctrl Pts',(15.0862248636567,8.24461078803355,2.85046016448875));
#8573=CARTESIAN_POINT('Ctrl Pts',(15.6007287737264,8.44313640296184,2.88750721366509));
#8574=CARTESIAN_POINT('Ctrl Pts',(16.115232683796,8.64166201789014,2.92455426284143));
#8575=CARTESIAN_POINT('Ctrl Pts',(16.5215906052904,9.12046146048677,2.96160131201777));
#8576=CARTESIAN_POINT('Ctrl Pts',(16.6338205503814,9.66039769069899,2.99864836119411));
#8577=CARTESIAN_POINT('Ctrl Pts',(16.7460504954725,10.2003339209112,3.03569541037045));
#8578=CARTESIAN_POINT('Ctrl Pts',(16.5641524641601,10.801406938739,3.07274245954679));
#8579=CARTESIAN_POINT('Ctrl Pts',(16.1713775896356,11.1885175058972,3.10978950872313));
#8580=CARTESIAN_POINT('Ctrl Pts',(15.7786027151111,11.5756280730554,3.14683655789947));
#8581=CARTESIAN_POINT('Ctrl Pts',(15.1749509973745,11.7487761895439,3.18388360707581));
#8582=CARTESIAN_POINT('Ctrl Pts',(14.6367018947022,11.6287153852114,3.22093065625215));
#8583=CARTESIAN_POINT('Ctrl Pts',(14.0984527920298,11.5086545808789,3.25797770542849));
#8584=CARTESIAN_POINT('Ctrl Pts',(13.6256063044218,11.0953848557254,3.29502475460483));
#8585=CARTESIAN_POINT('Ctrl Pts',(13.4345749220722,10.5780515934819,3.33207180378117));
#8586=CARTESIAN_POINT('Ctrl Pts',(13.3668387884629,10.3946149531724,3.34520799031751));
#8587=CARTESIAN_POINT('Ctrl Pts',(13.3345346524356,10.198094631663,3.35834417685386));
#8588=CARTESIAN_POINT('Ctrl Pts',(13.3358101889457,10.0011694310247,3.37148036339021));
#8589=CARTESIAN_POINT('Origin',(15.,10.,4.));
#8590=CARTESIAN_POINT('',(13.3357191812891,9.99878755125724,4.07148036339021));
#8591=CARTESIAN_POINT('',(13.3319678106811,9.99903395442804,3.8785196366098));
#8592=CARTESIAN_POINT('',(13.334,10.,4.));
#8593=CARTESIAN_POINT('Ctrl Pts',(13.3319678106811,9.99903395442804,3.8785196366098));
#8594=CARTESIAN_POINT('Ctrl Pts',(13.3353869165692,10.4944017554198,3.84527942973543));
#8595=CARTESIAN_POINT('Ctrl Pts',(13.5702060291847,10.9925841837293,3.81203922286105));
#8596=CARTESIAN_POINT('Ctrl Pts',(13.956288166515,11.3020614980076,3.77879901598667));
#8597=CARTESIAN_POINT('Ctrl Pts',(14.3865864490088,11.6469817725522,3.74175196681033));
#8598=CARTESIAN_POINT('Ctrl Pts',(15.0047785913624,11.7574988787253,3.70470491763399));
#8599=CARTESIAN_POINT('Ctrl Pts',(15.5279302703839,11.5830313217246,3.66765786845765));
#8600=CARTESIAN_POINT('Ctrl Pts',(16.0510819494053,11.4085637647238,3.63061081928131));
#8601=CARTESIAN_POINT('Ctrl Pts',(16.4791931650947,10.9491115445491,3.59356377010497));
#8602=CARTESIAN_POINT('Ctrl Pts',(16.6163258768942,10.4149568599639,3.55651672092863));
#8603=CARTESIAN_POINT('Ctrl Pts',(16.7534585886938,9.88080217537861,3.51946967175229));
#8604=CARTESIAN_POINT('Ctrl Pts',(16.5996127966036,9.27194502638277,3.48242262257595));
#8605=CARTESIAN_POINT('Ctrl Pts',(16.2252006784518,8.86704729424585,3.44537557339961));
#8606=CARTESIAN_POINT('Ctrl Pts',(15.8507885603,8.46214956210894,3.40832852422327));
#8607=CARTESIAN_POINT('Ctrl Pts',(15.2558101160866,8.26121124683096,3.37128147504694));
#8608=CARTESIAN_POINT('Ctrl Pts',(14.712575218255,8.35619784317566,3.3342344258706));
#8609=CARTESIAN_POINT('Ctrl Pts',(14.1693403204234,8.45118443952036,3.29718737669426));
#8610=CARTESIAN_POINT('Ctrl Pts',(13.6778489689736,8.84209594748775,3.26014032751791));
#8611=CARTESIAN_POINT('Ctrl Pts',(13.4630470397004,9.35001989740103,3.22309327834157));
#8612=CARTESIAN_POINT('Ctrl Pts',(13.3768997895452,9.55372501178734,3.20823539776431));
#8613=CARTESIAN_POINT('Ctrl Pts',(13.3352565386142,9.77625094550465,3.19337751718706));
#8614=CARTESIAN_POINT('Ctrl Pts',(13.3362901345243,9.99914721744613,3.1785196366098));
#8615=CARTESIAN_POINT('Ctrl Pts',(13.3358101889457,10.0011694310247,3.37148036339021));
#8616=CARTESIAN_POINT('Ctrl Pts',(13.3381319570023,9.64272054559026,3.3953912260302));
#8617=CARTESIAN_POINT('Ctrl Pts',(13.4517109778754,9.28293020158332,3.4193020886702));
#8618=CARTESIAN_POINT('Ctrl Pts',(13.6653761754273,8.99826222682056,3.44321295131019));
#8619=CARTESIAN_POINT('Ctrl Pts',(13.9964250882229,8.55720292173609,3.48026000048653));
#8620=CARTESIAN_POINT('Ctrl Pts',(14.5677391909053,8.29648111090055,3.51730704966287));
#8621=CARTESIAN_POINT('Ctrl Pts',(15.1178393123602,8.33542401321063,3.55435409883921));
#8622=CARTESIAN_POINT('Ctrl Pts',(15.6679394338151,8.37436691552071,3.59140114801555));
#8623=CARTESIAN_POINT('Ctrl Pts',(16.1968255740426,8.71297453097641,3.62844819719189));
#8624=CARTESIAN_POINT('Ctrl Pts',(16.4624370016316,9.1962728475463,3.66549524636823));
#8625=CARTESIAN_POINT('Ctrl Pts',(16.7280484292206,9.67957116411619,3.70254229554457));
#8626=CARTESIAN_POINT('Ctrl Pts',(16.7303851441713,10.3075601818003,3.7395893447209));
#8627=CARTESIAN_POINT('Ctrl Pts',(16.4683776782427,10.7928217412326,3.77663639389724));
#8628=CARTESIAN_POINT('Ctrl Pts',(16.2063702123141,11.278083300665,3.81368344307358));
#8629=CARTESIAN_POINT('Ctrl Pts',(15.6800185655062,11.6206174018456,3.85073049224993));
#8630=CARTESIAN_POINT('Ctrl Pts',(15.1302234816933,11.6636529578456,3.88777754142627));
#8631=CARTESIAN_POINT('Ctrl Pts',(14.5804283978804,11.7066885138457,3.92482459060261));
#8632=CARTESIAN_POINT('Ctrl Pts',(14.0071898770624,11.4502255246651,3.96187163977895));
#8633=CARTESIAN_POINT('Ctrl Pts',(13.6728678584929,11.011642030716,3.99891868895529));
#8634=CARTESIAN_POINT('Ctrl Pts',(13.4545961741777,10.7253002625409,4.02310591376693));
#8635=CARTESIAN_POINT('Ctrl Pts',(13.33816275372,10.3613295493415,4.04729313857857));
#8636=CARTESIAN_POINT('Ctrl Pts',(13.3357191812891,9.99878755125724,4.07148036339021));
#8637=CARTESIAN_POINT('Origin',(15.,10.,4.));
#8638=CARTESIAN_POINT('',(13.3314356817851,9.99950756868951,4.77148036339021));
#8639=CARTESIAN_POINT('',(13.3333640758576,10.0014616028283,4.5785196366098));
#8640=CARTESIAN_POINT('',(13.334,10.,4.));
#8641=CARTESIAN_POINT('Ctrl Pts',(13.3333640758576,10.0014616028283,4.5785196366098));
#8642=CARTESIAN_POINT('Ctrl Pts',(13.3323717044974,10.1096548526297,4.57127544063647));
#8643=CARTESIAN_POINT('Ctrl Pts',(13.342005436937,10.2176721573884,4.56403124466314));
#8644=CARTESIAN_POINT('Ctrl Pts',(13.3629079833276,10.3234629266178,4.55678704868981));
#8645=CARTESIAN_POINT('Ctrl Pts',(13.4698042720109,10.8644802934135,4.51973999951348));
#8646=CARTESIAN_POINT('Ctrl Pts',(13.8714174816763,11.3472663593339,4.48269295033713));
#8647=CARTESIAN_POINT('Ctrl Pts',(14.3839371853126,11.5508594856755,4.44564590116079));
#8648=CARTESIAN_POINT('Ctrl Pts',(14.896456888949,11.7544526120171,4.40859885198445));
#8649=CARTESIAN_POINT('Ctrl Pts',(15.5198830865563,11.6788527987799,4.37155180280811));
#8650=CARTESIAN_POINT('Ctrl Pts',(15.9688859313197,11.3586605860333,4.33450475363177));
#8651=CARTESIAN_POINT('Ctrl Pts',(16.417888776083,11.0384683732866,4.29745770445543));
#8652=CARTESIAN_POINT('Ctrl Pts',(16.6924682680023,10.4736837610304,4.26041065527909));
#8653=CARTESIAN_POINT('Ctrl Pts',(16.6669548014878,9.92279750168509,4.22336360610275));
#8654=CARTESIAN_POINT('Ctrl Pts',(16.6414413349734,9.37191124233978,4.18631655692641));
#8655=CARTESIAN_POINT('Ctrl Pts',(16.3158349100251,8.83492333590533,4.14926950775008));
#8656=CARTESIAN_POINT('Ctrl Pts',(15.8391591507847,8.55760253203077,4.11222245857374));
#8657=CARTESIAN_POINT('Ctrl Pts',(15.3624833915443,8.28028172815621,4.07517540939739));
#8658=CARTESIAN_POINT('Ctrl Pts',(14.7347382980116,8.26262802684153,4.03812836022105));
#8659=CARTESIAN_POINT('Ctrl Pts',(14.243230390291,8.5127211782015,4.00108131104471));
#8660=CARTESIAN_POINT('Ctrl Pts',(13.7517224825704,8.76281432956148,3.96403426186837));
#8661=CARTESIAN_POINT('Ctrl Pts',(13.3964517606618,9.2806543335961,3.92698721269204));
#8662=CARTESIAN_POINT('Ctrl Pts',(13.3400186110245,9.82923605707147,3.8899401635157));
#8663=CARTESIAN_POINT('Ctrl Pts',(13.3342197118936,9.88560664953272,3.88613332121373));
#8664=CARTESIAN_POINT('Ctrl Pts',(13.3315762367965,9.94230184361494,3.88232647891177));
#8665=CARTESIAN_POINT('Ctrl Pts',(13.3319678106811,9.99903395442804,3.8785196366098));
#8666=CARTESIAN_POINT('Ctrl Pts',(13.3357191812891,9.99878755125724,4.07148036339021));
#8667=CARTESIAN_POINT('Ctrl Pts',(13.3344199866718,9.80603181113007,4.08434018775491));
#8668=CARTESIAN_POINT('Ctrl Pts',(13.3653436581471,9.61367994289709,4.09720001211961));
#8669=CARTESIAN_POINT('Ctrl Pts',(13.4303165283821,9.43361398475765,4.1100598364843));
#8670=CARTESIAN_POINT('Ctrl Pts',(13.6174927331622,8.91487343146603,4.14710688566065));
#8671=CARTESIAN_POINT('Ctrl Pts',(14.0872506590436,8.49809632360041,4.18415393483699));
#8672=CARTESIAN_POINT('Ctrl Pts',(14.6245913894808,8.3740333046211,4.22120098401333));
#8673=CARTESIAN_POINT('Ctrl Pts',(15.161932119918,8.24997028564179,4.25824803318967));
#8674=CARTESIAN_POINT('Ctrl Pts',(15.7668556549109,8.41862135554878,4.295295082366));
#8675=CARTESIAN_POINT('Ctrl Pts',(16.1625004505648,8.80279825352266,4.33234213154234));
#8676=CARTESIAN_POINT('Ctrl Pts',(16.5581452462186,9.18697515149654,4.36938918071868));
#8677=CARTESIAN_POINT('Ctrl Pts',(16.7445113025333,9.7866778775373,4.40643622989502));
#8678=CARTESIAN_POINT('Ctrl Pts',(16.6363025596002,10.3274343488058,4.44348327907136));
#8679=CARTESIAN_POINT('Ctrl Pts',(16.5280938166672,10.8681908200742,4.4805303282477));
#8680=CARTESIAN_POINT('Ctrl Pts',(16.1253102744864,11.3500010365704,4.51757737742405));
#8681=CARTESIAN_POINT('Ctrl Pts',(15.612297998127,11.5523499865775,4.55462442660038));
#8682=CARTESIAN_POINT('Ctrl Pts',(15.0992857217675,11.7546989365846,4.59167147577672));
#8683=CARTESIAN_POINT('Ctrl Pts',(14.4760447112292,11.6775866201028,4.62871852495306));
#8684=CARTESIAN_POINT('Ctrl Pts',(14.0278200568663,11.3563058200469,4.6657655741294));
#8685=CARTESIAN_POINT('Ctrl Pts',(13.6014795346479,11.0507112421021,4.70100383721634));
#8686=CARTESIAN_POINT('Ctrl Pts',(13.3334825638361,10.5242087120345,4.73624210030327));
#8687=CARTESIAN_POINT('Ctrl Pts',(13.3314356817851,9.99950756868951,4.77148036339021));
#8688=CARTESIAN_POINT('Origin',(15.,10.,4.));
#8689=CARTESIAN_POINT('',(13.3342680156708,10.0015218068924,5.47148036339021));
#8690=CARTESIAN_POINT('',(13.3367225736456,10.0000562476499,5.2785196366098));
#8691=CARTESIAN_POINT('',(13.334,10.,4.));
#8692=CARTESIAN_POINT('Ctrl Pts',(13.3367225736456,10.0000562476499,5.2785196366098));
#8693=CARTESIAN_POINT('Ctrl Pts',(13.3366398710265,10.2746976433381,5.26022440236118));
#8694=CARTESIAN_POINT('Ctrl Pts',(13.4008957839674,10.5493026139045,5.24192916811255));
#8695=CARTESIAN_POINT('Ctrl Pts',(13.5297031058243,10.7892563454686,5.22363393386393));
#8696=CARTESIAN_POINT('Ctrl Pts',(13.7905322989496,11.2751521570498,5.18658688468759));
#8697=CARTESIAN_POINT('Ctrl Pts',(14.3160511791024,11.618962369561,5.14953983551125));
#8698=CARTESIAN_POINT('Ctrl Pts',(14.8657401432864,11.6633318450802,5.11249278633491));
#8699=CARTESIAN_POINT('Ctrl Pts',(15.4154291074705,11.7077013205994,5.07544573715857));
#8700=CARTESIAN_POINT('Ctrl Pts',(15.9892881556857,11.4526300591266,5.03839868798224));
#8701=CARTESIAN_POINT('Ctrl Pts',(16.3246733455339,11.014859134846,5.00135163880589));
#8702=CARTESIAN_POINT('Ctrl Pts',(16.6600585353821,10.5770882105654,4.96430458962956));
#8703=CARTESIAN_POINT('Ctrl Pts',(16.7569698668632,9.95661762347699,4.92725754045321));
#8704=CARTESIAN_POINT('Ctrl Pts',(16.5710529393037,9.43742449587025,4.89021049127687));
#8705=CARTESIAN_POINT('Ctrl Pts',(16.3851360117441,8.91823136826352,4.85316344210053));
#8706=CARTESIAN_POINT('Ctrl Pts',(15.9163908251438,8.50031570013841,4.8161163929242));
#8707=CARTESIAN_POINT('Ctrl Pts',(15.3793527852933,8.37494923148702,4.77906934374785));
#8708=CARTESIAN_POINT('Ctrl Pts',(14.8423147454429,8.24958276283564,4.74202229457151));
#8709=CARTESIAN_POINT('Ctrl Pts',(14.2369838523423,8.41676549365797,4.70497524539517));
#8710=CARTESIAN_POINT('Ctrl Pts',(13.8404080896426,8.79998119290459,4.66792819621883));
#8711=CARTESIAN_POINT('Ctrl Pts',(13.5213789226136,9.10826272905,4.63812534301582));
#8712=CARTESIAN_POINT('Ctrl Pts',(13.3374467232736,9.55635112358934,4.60832248981281));
#8713=CARTESIAN_POINT('Ctrl Pts',(13.3333640758576,10.0014616028283,4.5785196366098));
#8714=CARTESIAN_POINT('Ctrl Pts',(13.3314356817851,9.99950756868951,4.77148036339021));
#8715=CARTESIAN_POINT('Ctrl Pts',(13.3313306149783,9.97257456898871,4.77328914947961));
#8716=CARTESIAN_POINT('Ctrl Pts',(13.3319262698781,9.94564631555734,4.77509793556902));
#8717=CARTESIAN_POINT('Ctrl Pts',(13.3332371996276,9.91875292850695,4.77690672165842));
#8718=CARTESIAN_POINT('Ctrl Pts',(13.3600872949395,9.3679301206525,4.81395377083476));
#8719=CARTESIAN_POINT('Ctrl Pts',(13.6869957837509,8.83173378857331,4.8510008200111));
#8720=CARTESIAN_POINT('Ctrl Pts',(14.1643431130298,8.55557039402238,4.88804786918744));
#8721=CARTESIAN_POINT('Ctrl Pts',(14.6416904423087,8.27940699947144,4.92509491836378));
#8722=CARTESIAN_POINT('Ctrl Pts',(15.2694766120551,8.26327654244874,4.96214196754013));
#8723=CARTESIAN_POINT('Ctrl Pts',(15.7603763023923,8.51456161419294,4.99918901671647));
#8724=CARTESIAN_POINT('Ctrl Pts',(16.2512759927295,8.76584668593715,5.03623606589281));
#8725=CARTESIAN_POINT('Ctrl Pts',(16.6052892036575,9.28454728644825,5.07328311506914));
#8726=CARTESIAN_POINT('Ctrl Pts',(16.6603910866373,9.83326440464277,5.11033016424548));
#8727=CARTESIAN_POINT('Ctrl Pts',(16.7154929696171,10.3819815228373,5.14737721342182));
#8728=CARTESIAN_POINT('Ctrl Pts',(16.4716835246487,10.9607151587152,5.18442426259816));
#8729=CARTESIAN_POINT('Ctrl Pts',(16.0405495150863,11.3045903672043,5.2214713117745));
#8730=CARTESIAN_POINT('Ctrl Pts',(15.6094155055239,11.6484655756935,5.25851836095084));
#8731=CARTESIAN_POINT('Ctrl Pts',(14.9909569313674,11.7574823567937,5.29556541012719));
#8732=CARTESIAN_POINT('Ctrl Pts',(14.4682300563887,11.5817458853773,5.33261245930353));
#8733=CARTESIAN_POINT('Ctrl Pts',(13.94550318141,11.4060094139609,5.36965950847987));
#8734=CARTESIAN_POINT('Ctrl Pts',(13.518508005609,10.9455196900277,5.4067065576562));
#8735=CARTESIAN_POINT('Ctrl Pts',(13.3826717801281,10.4110337562418,5.44375360683254));
#8736=CARTESIAN_POINT('Ctrl Pts',(13.3487842592651,10.2776937494211,5.45299585901843));
#8737=CARTESIAN_POINT('Ctrl Pts',(13.3330175869468,10.1397484432952,5.46223811120432));
#8738=CARTESIAN_POINT('Ctrl Pts',(13.3342680156708,10.0015218068924,5.47148036339021));
#8739=CARTESIAN_POINT('Origin',(15.,10.,4.));
#8740=CARTESIAN_POINT('',(13.3366211461937,9.99956957717865,6.17148036339021));
#8741=CARTESIAN_POINT('',(13.3335705647763,9.99850933114582,5.9785196366098));
#8742=CARTESIAN_POINT('',(13.334,10.,4.));
#8743=CARTESIAN_POINT('Ctrl Pts',(13.3335705647763,9.99850933114582,5.9785196366098));
#8744=CARTESIAN_POINT('Ctrl Pts',(13.3376165322179,10.4369404297967,5.94917336408588));
#8745=CARTESIAN_POINT('Ctrl Pts',(13.5153563455701,10.8782736326066,5.91982709156196));
#8746=CARTESIAN_POINT('Ctrl Pts',(13.8257421415539,11.1856715455913,5.89048081903805));
#8747=CARTESIAN_POINT('Ctrl Pts',(14.2175764993273,11.573733967821,5.85343376986171));
#8748=CARTESIAN_POINT('Ctrl Pts',(14.8208062179761,11.7483462850056,5.81638672068537));
#8749=CARTESIAN_POINT('Ctrl Pts',(15.3593449820839,11.6295918879259,5.77933967150903));
#8750=CARTESIAN_POINT('Ctrl Pts',(15.8978837461918,11.5108374908461,5.7422926223327));
#8751=CARTESIAN_POINT('Ctrl Pts',(16.3717315557589,11.098716379502,5.70524557315635));
#8752=CARTESIAN_POINT('Ctrl Pts',(16.5640176341788,10.5818482415203,5.66819852398001));
#8753=CARTESIAN_POINT('Ctrl Pts',(16.7563037125987,10.0649801035386,5.63115147480367));
#8754=CARTESIAN_POINT('Ctrl Pts',(16.6670280598714,9.44336493891926,5.59410442562733));
#8755=CARTESIAN_POINT('Ctrl Pts',(16.3370503780492,9.0015037195829,5.55705737645099));
#8756=CARTESIAN_POINT('Ctrl Pts',(16.0070726962269,8.55964250024654,5.52001032727465));
#8757=CARTESIAN_POINT('Ctrl Pts',(15.4363929853096,8.29753522619313,5.48296327809831));
#8758=CARTESIAN_POINT('Ctrl Pts',(14.8862000675362,8.33514321590732,5.44591622892197));
#8759=CARTESIAN_POINT('Ctrl Pts',(14.3360071497627,8.37275120562152,5.40886917974563));
#8760=CARTESIAN_POINT('Ctrl Pts',(13.8063010251331,8.71007445910332,5.37182213056929));
#8761=CARTESIAN_POINT('Ctrl Pts',(13.5395177158672,9.1927267911698,5.33477508139295));
#8762=CARTESIAN_POINT('Ctrl Pts',(13.4044820962327,9.43702714454645,5.31602326646523));
#8763=CARTESIAN_POINT('Ctrl Pts',(13.3368073402131,9.71856082903702,5.29727145153751));
#8764=CARTESIAN_POINT('Ctrl Pts',(13.3367225736456,10.0000562476499,5.2785196366098));
#8765=CARTESIAN_POINT('Ctrl Pts',(13.3342680156708,10.0015218068924,5.47148036339021));
#8766=CARTESIAN_POINT('Ctrl Pts',(13.3380298603082,9.58567472908586,5.49928516038066));
#8767=CARTESIAN_POINT('Ctrl Pts',(13.4958089693912,9.16728140562092,5.52708995737111));
#8768=CARTESIAN_POINT('Ctrl Pts',(13.7775518139329,8.86407757611185,5.55489475436156));
#8769=CARTESIAN_POINT('Ctrl Pts',(14.1529453483797,8.4600894734066,5.5919418035379));
#8770=CARTESIAN_POINT('Ctrl Pts',(14.7484096924343,8.26059541163487,5.62898885271425));
#8771=CARTESIAN_POINT('Ctrl Pts',(15.2914125868251,8.35689987529541,5.66603590189058));
#8772=CARTESIAN_POINT('Ctrl Pts',(15.834415481216,8.45320433895594,5.70308295106692));
#8773=CARTESIAN_POINT('Ctrl Pts',(16.3249569259433,8.84530732804875,5.74013000024326));
#8774=CARTESIAN_POINT('Ctrl Pts',(16.5385257988885,9.35375106326425,5.7771770494196));
#8775=CARTESIAN_POINT('Ctrl Pts',(16.7520946718337,9.86219479847975,5.81422409859594));
#8776=CARTESIAN_POINT('Ctrl Pts',(16.6886909729969,10.4869792798179,5.85127114777229));
#8777=CARTESIAN_POINT('Ctrl Pts',(16.3773333216744,10.9421529858403,5.88831819694863));
#8778=CARTESIAN_POINT('Ctrl Pts',(16.0659756703518,11.3973266918625,5.92536524612497));
#8779=CARTESIAN_POINT('Ctrl Pts',(15.5066640665436,11.6828896225689,5.9624122953013));
#8780=CARTESIAN_POINT('Ctrl Pts',(14.9553843754809,11.6681452986554,5.99945934447764));
#8781=CARTESIAN_POINT('Ctrl Pts',(14.4041046844183,11.6534009747418,6.03650639365398));
#8782=CARTESIAN_POINT('Ctrl Pts',(13.8608569061013,11.3383493962082,6.07355344283033));
#8783=CARTESIAN_POINT('Ctrl Pts',(13.5742748086562,10.8671833862294,6.11060049200666));
#8784=CARTESIAN_POINT('Ctrl Pts',(13.4172935139586,10.6090924205921,6.13089378246785));
#8785=CARTESIAN_POINT('Ctrl Pts',(13.3373254782368,10.3041588809966,6.15118707292903));
#8786=CARTESIAN_POINT('Ctrl Pts',(13.3366211461937,9.99956957717865,6.17148036339021));
#8787=CARTESIAN_POINT('Origin',(15.,10.,4.));
#8788=CARTESIAN_POINT('',(13.3326898978632,9.99870038716915,6.87148036339021));
#8789=CARTESIAN_POINT('',(13.3318213113649,10.0008675364682,6.6785196366098));
#8790=CARTESIAN_POINT('',(13.334,10.,4.));
#8791=CARTESIAN_POINT('Ctrl Pts',(13.3318213113649,10.0008675364682,6.6785196366098));
#8792=CARTESIAN_POINT('Ctrl Pts',(13.3315052103317,10.0507838401085,6.67516937498693));
#8793=CARTESIAN_POINT('Ctrl Pts',(13.3335514732033,10.1006738678638,6.67181911336406));
#8794=CARTESIAN_POINT('Ctrl Pts',(13.3380445549174,10.1503425512859,6.66846885174119));
#8795=CARTESIAN_POINT('Ctrl Pts',(13.3877288595927,10.6995767199555,6.63142180256485));
#8796=CARTESIAN_POINT('Ctrl Pts',(13.7366062926716,11.2217452545238,6.59437475338851));
#8797=CARTESIAN_POINT('Ctrl Pts',(14.2250023217333,11.4778622839724,6.55732770421217));
#8798=CARTESIAN_POINT('Ctrl Pts',(14.713398350795,11.7339793134211,6.52028065503583));
#8799=CARTESIAN_POINT('Ctrl Pts',(15.3413129758397,11.7240448377502,6.48323360585949));
#8800=CARTESIAN_POINT('Ctrl Pts',(15.8213622031389,11.4526054920116,6.44618655668315));
#8801=CARTESIAN_POINT('Ctrl Pts',(16.3014114304382,11.181166146273,6.40913950750681));
#8802=CARTESIAN_POINT('Ctrl Pts',(16.633595259992,10.6482219304667,6.37209245833047));
#8803=CARTESIAN_POINT('Ctrl Pts',(16.665879658905,10.0976909688753,6.33504540915413));
#8804=CARTESIAN_POINT('Ctrl Pts',(16.6981640578181,9.54716000728396,6.29799835997779));
#8805=CARTESIAN_POINT('Ctrl Pts',(16.4305490260904,8.9790422999075,6.26095131080145));
#8806=CARTESIAN_POINT('Ctrl Pts',(15.9855167048731,8.65335404348968,6.22390426162511));
#8807=CARTESIAN_POINT('Ctrl Pts',(15.5404843836558,8.32766578707186,6.18685721244877));
#8808=CARTESIAN_POINT('Ctrl Pts',(14.9180347729489,8.24440698161268,6.14981016327243));
#8809=CARTESIAN_POINT('Ctrl Pts',(14.4030507388859,8.44168356099275,6.11276311409609));
#8810=CARTESIAN_POINT('Ctrl Pts',(13.8880667048228,8.63896014037284,6.07571606491975));
#8811=CARTESIAN_POINT('Ctrl Pts',(13.4805482474035,9.11677210459218,6.03866901574341));
#8812=CARTESIAN_POINT('Ctrl Pts',(13.367008517143,9.65643435033934,6.00162196656707));
#8813=CARTESIAN_POINT('Ctrl Pts',(13.3434076063187,9.76861112324408,5.99392118991465));
#8814=CARTESIAN_POINT('Ctrl Pts',(13.3325088595262,9.88346030863584,5.98622041326222));
#8815=CARTESIAN_POINT('Ctrl Pts',(13.3335705647763,9.99850933114582,5.9785196366098));
#8816=CARTESIAN_POINT('Ctrl Pts',(13.3366211461937,9.99956957717865,6.17148036339021));
#8817=CARTESIAN_POINT('Ctrl Pts',(13.3360396629134,9.74810637986497,6.18823412210536));
#8818=CARTESIAN_POINT('Ctrl Pts',(13.3894830746076,9.49687780824835,6.20498788082052));
#8819=CARTESIAN_POINT('Ctrl Pts',(13.4982177136245,9.27243602933048,6.22174163953568));
#8820=CARTESIAN_POINT('Ctrl Pts',(13.7386591326111,8.77613512383438,6.25878868871202));
#8821=CARTESIAN_POINT('Ctrl Pts',(14.2494583871574,8.41081375426625,6.29583573788837));
#8822=CARTESIAN_POINT('Ctrl Pts',(14.7968327516103,8.34367207785079,6.33288278706471));
#8823=CARTESIAN_POINT('Ctrl Pts',(15.3442071160632,8.27653040143534,6.36992983624105));
#8824=CARTESIAN_POINT('Ctrl Pts',(15.9281565904228,8.50756841817255,6.40697688541738));
#8825=CARTESIAN_POINT('Ctrl Pts',(16.2814190520273,8.93104500588939,6.44402393459372));
#8826=CARTESIAN_POINT('Ctrl Pts',(16.6346815136318,9.35452159360624,6.48107098377006));
#8827=CARTESIAN_POINT('Ctrl Pts',(16.7572569624813,9.97043675230272,6.51811803294641));
#8828=CARTESIAN_POINT('Ctrl Pts',(16.5930450226178,10.4968974925493,6.55516508212274));
#8829=CARTESIAN_POINT('Ctrl Pts',(16.4288330827542,11.0233582327959,6.59221213129908));
#8830=CARTESIAN_POINT('Ctrl Pts',(15.9778337541777,11.4603645545926,6.62925918047542));
#8831=CARTESIAN_POINT('Ctrl Pts',(15.4464605454363,11.6079088474927,6.66630622965176));
#8832=CARTESIAN_POINT('Ctrl Pts',(14.9150873366949,11.7554531403928,6.70335327882809));
#8833=CARTESIAN_POINT('Ctrl Pts',(14.3033402477887,11.6135354043964,6.74040032800444));
#8834=CARTESIAN_POINT('Ctrl Pts',(13.891203767925,11.2471055880722,6.77744737718078));
#8835=CARTESIAN_POINT('Ctrl Pts',(13.5425082146664,10.9370809875421,6.80879170591726));
#8836=CARTESIAN_POINT('Ctrl Pts',(13.336700189492,10.4663436055774,6.84013603465374));
#8837=CARTESIAN_POINT('Ctrl Pts',(13.3326898978632,9.99870038716915,6.87148036339021));
#8838=CARTESIAN_POINT('Origin',(15.,10.,4.));
#8839=CARTESIAN_POINT('',(13.3325428889984,10.0012066618994,7.57148036339021));
#8840=CARTESIAN_POINT('',(13.3361815072522,10.0009395500142,7.3785196366098));
#8841=CARTESIAN_POINT('',(13.334,10.,4.));
#8842=CARTESIAN_POINT('',(16.2690708798524,11.0793586530485,8.));
#8843=CARTESIAN_POINT('Ctrl Pts',(13.3325428889984,10.0012066618994,7.57148036339021));
#8844=CARTESIAN_POINT('Ctrl Pts',(13.336490896492,9.52850371015197,7.60317909473112));
#8845=CARTESIAN_POINT('Ctrl Pts',(13.5475479048343,9.05282868422974,7.63487782607203));
#8846=CARTESIAN_POINT('Ctrl Pts',(13.9031583859685,8.74254052399572,7.66657655741294));
#8847=CARTESIAN_POINT('Ctrl Pts',(14.3187686777658,8.37989948933103,7.70362360658928));
#8848=CARTESIAN_POINT('Ctrl Pts',(14.9318266387037,8.24316275503293,7.74067065576562));
#8849=CARTESIAN_POINT('Ctrl Pts',(15.4617848325985,8.39611213748269,7.77771770494196));
#8850=CARTESIAN_POINT('Ctrl Pts',(15.9917430264934,8.54906151993244,7.8147647541183));
#8851=CARTESIAN_POINT('Ctrl Pts',(16.4386014533451,8.99169701913006,7.85181180329464));
#8852=CARTESIAN_POINT('Ctrl Pts',(16.5976641540082,9.51876914569494,7.88885885247098));
#8853=CARTESIAN_POINT('Ctrl Pts',(16.7567268546712,10.0458412722598,7.92590590164732));
#8854=CARTESIAN_POINT('Ctrl Pts',(16.6279938291456,10.657350026192,7.96295295082366));
#8855=CARTESIAN_POINT('Ctrl Pts',(16.2690708798524,11.0793586530485,8.));
#8856=CARTESIAN_POINT('',(13.7285471518004,11.0812363616735,8.));
#8857=CARTESIAN_POINT('Origin',(15.,10.,8.));
#8858=CARTESIAN_POINT('Ctrl Pts',(13.7285463279864,11.0812370110871,8.));
#8859=CARTESIAN_POINT('Ctrl Pts',(14.0794405795174,11.4928283988345,7.96367382485347));
#8860=CARTESIAN_POINT('Ctrl Pts',(14.6494732486073,11.7187788632783,7.92734764970694));
#8861=CARTESIAN_POINT('Ctrl Pts',(15.1869067772186,11.6581102602073,7.89102147456041));
#8862=CARTESIAN_POINT('Ctrl Pts',(15.7350053943497,11.5962377203,7.85397442538407));
#8863=CARTESIAN_POINT('Ctrl Pts',(16.2491982074161,11.2362576290369,7.81692737620773));
#8864=CARTESIAN_POINT('Ctrl Pts',(16.4944802724612,10.7424222627658,7.77988032703139));
#8865=CARTESIAN_POINT('Ctrl Pts',(16.7397623375063,10.2485868964947,7.74283327785505));
#8866=CARTESIAN_POINT('Ctrl Pts',(16.71613365453,9.6208962552156,7.70578622867871));
#8867=CARTESIAN_POINT('Ctrl Pts',(16.4342383674864,9.14688996574335,7.66873917950237));
#8868=CARTESIAN_POINT('Ctrl Pts',(16.1523430804427,8.6728836762711,7.63169213032603));
#8869=CARTESIAN_POINT('Ctrl Pts',(15.6121811893316,8.35256173860573,7.59464508114969));
#8870=CARTESIAN_POINT('Ctrl Pts',(15.0610619107686,8.3323961960037,7.55759803197335));
#8871=CARTESIAN_POINT('Ctrl Pts',(14.5099426322055,8.31223065340166,7.52055098279701));
#8872=CARTESIAN_POINT('Ctrl Pts',(13.9478659661905,8.59222150586297,7.48350393362067));
#8873=CARTESIAN_POINT('Ctrl Pts',(13.6320379889576,9.04429107975044,7.44645688444433));
#8874=CARTESIAN_POINT('Ctrl Pts',(13.4389818253369,9.32062764242292,7.42381113516615));
#8875=CARTESIAN_POINT('Ctrl Pts',(13.3379367298706,9.66126159097544,7.40116538588797));
#8876=CARTESIAN_POINT('Ctrl Pts',(13.3361815072522,10.0009395500142,7.3785196366098));
#8877=CARTESIAN_POINT('Origin',(-15.,10.,4.));
#8878=CARTESIAN_POINT('',(-16.6671909719797,10.0013492775649,0.571480363390205));
#8879=CARTESIAN_POINT('',(-16.6635931317265,10.000664586652,0.378519636609791));
#8880=CARTESIAN_POINT('',(-16.666,10.,4.));
#8881=CARTESIAN_POINT('',(-13.3882904778579,9.57816067485776,0.));
#8882=CARTESIAN_POINT('Ctrl Pts',(-16.6635931317265,10.000664586652,0.378519636609791));
#8883=CARTESIAN_POINT('Ctrl Pts',(-16.6645712763617,10.2261440155287,0.363487571935547));
#8884=CARTESIAN_POINT('Ctrl Pts',(-16.6219037410329,10.4512893271606,0.348455507261303));
#8885=CARTESIAN_POINT('Ctrl Pts',(-16.5338109814408,10.6570298951176,0.333423442587058));
#8886=CARTESIAN_POINT('Ctrl Pts',(-16.3167032941462,11.1640847211743,0.296376393410719));
#8887=CARTESIAN_POINT('Ctrl Pts',(-15.8236858537848,11.5532764409388,0.259329344234379));
#8888=CARTESIAN_POINT('Ctrl Pts',(-15.279847491745,11.6454139691312,0.22228229505804));
#8889=CARTESIAN_POINT('Ctrl Pts',(-14.7360091297051,11.7375514973235,0.1852352458817));
#8890=CARTESIAN_POINT('Ctrl Pts',(-14.1413498459868,11.5326348339436,0.148188196705361));
#8891=CARTESIAN_POINT('Ctrl Pts',(-13.7693512524429,11.1267739948468,0.11114114752902));
#8892=CARTESIAN_POINT('Ctrl Pts',(-13.397352658899,10.72091315575,0.0740940983526811));
#8893=CARTESIAN_POINT('Ctrl Pts',(-13.2480147555294,10.1141081409362,0.0370470491763408));
#8894=CARTESIAN_POINT('Ctrl Pts',(-13.3882904778579,9.57816067485778,1.59594559789866E-15));
#8895=CARTESIAN_POINT('',(-15.675077185675,8.47690223774664,0.));
#8896=CARTESIAN_POINT('Origin',(-15.,10.,0.));
#8897=CARTESIAN_POINT('Ctrl Pts',(-15.676409110153,8.47417610875464,5.20417042793042E-17));
#8898=CARTESIAN_POINT('Ctrl Pts',(-15.1816815462137,8.25559244463078,0.0363261751465299));
#8899=CARTESIAN_POINT('Ctrl Pts',(-14.5700634796721,8.29934581648217,0.0726523502930598));
#8900=CARTESIAN_POINT('Ctrl Pts',(-14.1121756761023,8.58718997742447,0.10897852543959));
#8901=CARTESIAN_POINT('Ctrl Pts',(-13.6452013275045,8.88074625585282,0.14602557461593));
#8902=CARTESIAN_POINT('Ctrl Pts',(-13.338119175407,9.42817715635473,0.18307262379227));
#8903=CARTESIAN_POINT('Ctrl Pts',(-13.3313948226923,9.97953138687446,0.22011967296861));
#8904=CARTESIAN_POINT('Ctrl Pts',(-13.3246704699776,10.5308856173942,0.257166722144951));
#8905=CARTESIAN_POINT('Ctrl Pts',(-13.6183039166457,11.0861631779317,0.294213771321291));
#8906=CARTESIAN_POINT('Ctrl Pts',(-14.0779464201314,11.3909182993711,0.331260820497631));
#8907=CARTESIAN_POINT('Ctrl Pts',(-14.537588923617,11.6956734208104,0.368307869673971));
#8908=CARTESIAN_POINT('Ctrl Pts',(-15.1632404839201,11.7499061031516,0.405354918850311));
#8909=CARTESIAN_POINT('Ctrl Pts',(-15.6685313154342,11.5289529396842,0.442401968026651));
#8910=CARTESIAN_POINT('Ctrl Pts',(-16.1738221469483,11.3079997762168,0.479449017202991));
#8911=CARTESIAN_POINT('Ctrl Pts',(-16.5587522496733,10.8118607669409,0.516496066379331));
#8912=CARTESIAN_POINT('Ctrl Pts',(-16.6471577882404,10.2675275099722,0.55354311555567));
#8913=CARTESIAN_POINT('Ctrl Pts',(-16.6614256997248,10.1796766936732,0.559522198167182));
#8914=CARTESIAN_POINT('Ctrl Pts',(-16.6679699620053,10.0905705497967,0.565501280778694));
#8915=CARTESIAN_POINT('Ctrl Pts',(-16.6671909719797,10.0013492775649,0.571480363390205));
#8916=CARTESIAN_POINT('Origin',(-15.,10.,4.));
#8917=CARTESIAN_POINT('',(-16.6633491135953,10.0003647770189,1.27148036339021));
#8918=CARTESIAN_POINT('',(-16.6649907195691,9.99856203207469,1.07851963660979));
#8919=CARTESIAN_POINT('',(-16.666,10.,4.));
#8920=CARTESIAN_POINT('Ctrl Pts',(-16.6649907195691,9.99856203207469,1.07851963660979));
#8921=CARTESIAN_POINT('Ctrl Pts',(-16.6617723069357,10.3890986075708,1.05243653366026));
#8922=CARTESIAN_POINT('Ctrl Pts',(-16.5246077087442,10.7816701084545,1.02635343071072));
#8923=CARTESIAN_POINT('Ctrl Pts',(-16.2737774517755,11.0780444210991,1.00027032776118));
#8924=CARTESIAN_POINT('Ctrl Pts',(-15.9175115242587,11.4989986977583,0.963223278584839));
#8925=CARTESIAN_POINT('Ctrl Pts',(-15.3319382306252,11.7258862342935,0.9261762294085));
#8926=CARTESIAN_POINT('Ctrl Pts',(-14.7850529907541,11.654845590621,0.88912918023216));
#8927=CARTESIAN_POINT('Ctrl Pts',(-14.238167750883,11.5838049469485,0.85208213105582));
#8928=CARTESIAN_POINT('Ctrl Pts',(-13.7299705647742,11.2148361230683,0.815035081879479));
#8929=CARTESIAN_POINT('Ctrl Pts',(-13.4930724270708,10.7168466467109,0.77798803270314));
#8930=CARTESIAN_POINT('Ctrl Pts',(-13.2561742893673,10.2188571703535,0.7409409835268));
#8931=CARTESIAN_POINT('Ctrl Pts',(-13.2905752000691,9.59184704151887,0.703893934350459));
#8932=CARTESIAN_POINT('Ctrl Pts',(-13.5804933523073,9.12271316008998,0.666846885174119));
#8933=CARTESIAN_POINT('Ctrl Pts',(-13.8704115045454,8.6535792786611,0.62979983599778));
#8934=CARTESIAN_POINT('Ctrl Pts',(-14.4158468983198,8.34232164463794,0.59275278682144));
#8935=CARTESIAN_POINT('Ctrl Pts',(-14.9672366360564,8.33153869325115,0.5557057376451));
#8936=CARTESIAN_POINT('Ctrl Pts',(-15.5186263737931,8.32075574186434,0.518658688468759));
#8937=CARTESIAN_POINT('Ctrl Pts',(-16.075970455492,8.61044747311391,0.481611639292419));
#8938=CARTESIAN_POINT('Ctrl Pts',(-16.3840435292275,9.06775230491307,0.444564590116079));
#8939=CARTESIAN_POINT('Ctrl Pts',(-16.5671140866562,9.33950293036427,0.422549605613983));
#8940=CARTESIAN_POINT('Ctrl Pts',(-16.662160604695,9.67044207631607,0.400534621111887));
#8941=CARTESIAN_POINT('Ctrl Pts',(-16.6635931317265,10.000664586652,0.378519636609791));
#8942=CARTESIAN_POINT('Ctrl Pts',(-16.6671909719797,10.0013492775649,0.571480363390205));
#8943=CARTESIAN_POINT('Ctrl Pts',(-16.6631432546885,9.53774579812301,0.602548329955034));
#8944=CARTESIAN_POINT('Ctrl Pts',(-16.4613710095151,9.07103390472509,0.633616296519862));
#8945=CARTESIAN_POINT('Ctrl Pts',(-16.1180469662142,8.76117513340022,0.66468426308469));
#8946=CARTESIAN_POINT('Ctrl Pts',(-15.7086496312117,8.39168351845854,0.70173131226103));
#8947=CARTESIAN_POINT('Ctrl Pts',(-15.0979739867974,8.24522779323672,0.73877836143737));
#8948=CARTESIAN_POINT('Ctrl Pts',(-14.5655171497087,8.3888161695707,0.77582541061371));
#8949=CARTESIAN_POINT('Ctrl Pts',(-14.03306031262,8.53240454590468,0.81287245979005));
#8950=CARTESIAN_POINT('Ctrl Pts',(-13.5788222828569,8.96603702379445,0.84991950896639));
#8951=CARTESIAN_POINT('Ctrl Pts',(-13.4106973070842,9.49125977655298,0.88696655814273));
#8952=CARTESIAN_POINT('Ctrl Pts',(-13.2425723313114,10.0164825293115,0.92401360731907));
#8953=CARTESIAN_POINT('Ctrl Pts',(-13.3605604095291,10.6332955569388,0.961060656495409));
#8954=CARTESIAN_POINT('Ctrl Pts',(-13.7106615151752,11.0593899574044,0.998107705671749));
#8955=CARTESIAN_POINT('Ctrl Pts',(-14.0607626208212,11.48548435787,1.03515475484809));
#8956=CARTESIAN_POINT('Ctrl Pts',(-14.6429767538956,11.7208601311739,1.07220180402443));
#8957=CARTESIAN_POINT('Ctrl Pts',(-15.1908356100492,11.6577934174094,1.10924885320077));
#8958=CARTESIAN_POINT('Ctrl Pts',(-15.7386944662028,11.5947267036449,1.14629590237711));
#8959=CARTESIAN_POINT('Ctrl Pts',(-16.2521980454357,11.2332175028119,1.18334295155345));
#8960=CARTESIAN_POINT('Ctrl Pts',(-16.4963261193042,10.7387198928195,1.22039000072979));
#8961=CARTESIAN_POINT('Ctrl Pts',(-16.6085491087805,10.5114047823413,1.2374201216166));
#8962=CARTESIAN_POINT('Ctrl Pts',(-16.663849289669,10.2559873626026,1.2544502425034));
#8963=CARTESIAN_POINT('Ctrl Pts',(-16.6633491135953,10.0003647770189,1.27148036339021));
#8964=CARTESIAN_POINT('Origin',(-15.,10.,4.));
#8965=CARTESIAN_POINT('',(-16.6658557594656,9.99847620480149,1.97148036339021));
#8966=CARTESIAN_POINT('',(-16.6687417212197,10.000024262485,1.77851963660979));
#8967=CARTESIAN_POINT('',(-16.666,10.,4.));
#8968=CARTESIAN_POINT('Ctrl Pts',(-16.6687412413332,10.0000242582383,1.77851963660979));
#8969=CARTESIAN_POINT('Ctrl Pts',(-16.6688598782876,10.5527978471161,1.74138549538496));
#8970=CARTESIAN_POINT('Ctrl Pts',(-16.3668274413062,11.1054588942412,1.70425135416013));
#8971=CARTESIAN_POINT('Ctrl Pts',(-15.9017010292556,11.4041487895867,1.6671172129353));
#8972=CARTESIAN_POINT('Ctrl Pts',(-15.4376654950521,11.7021381566853,1.63007016375896));
#8973=CARTESIAN_POINT('Ctrl Pts',(-14.8113016216914,11.7473462740701,1.59302311458262));
#8974=CARTESIAN_POINT('Ctrl Pts',(-14.3092835852333,11.5190819120405,1.55597606540628));
#8975=CARTESIAN_POINT('Ctrl Pts',(-13.8072655487753,11.2908175500109,1.51892901622994));
#8976=CARTESIAN_POINT('Ctrl Pts',(-13.42959334922,10.789080708567,1.4818819670536));
#8977=CARTESIAN_POINT('Ctrl Pts',(-13.3491204486805,10.2435071350204,1.44483491787726));
#8978=CARTESIAN_POINT('Ctrl Pts',(-13.268647548141,9.69793356147377,1.40778786870092));
#8979=CARTESIAN_POINT('Ctrl Pts',(-13.4853739466174,9.10852325582452,1.37074081952458));
#8980=CARTESIAN_POINT('Ctrl Pts',(-13.9001075538765,8.7450362812419,1.33369377034824));
#8981=CARTESIAN_POINT('Ctrl Pts',(-14.3148411611356,8.38154930665928,1.2966467211719));
#8982=CARTESIAN_POINT('Ctrl Pts',(-14.9275819771775,8.24398566314329,1.25959967199556));
#8983=CARTESIAN_POINT('Ctrl Pts',(-15.4578920033439,8.39530818992637,1.22255262281922));
#8984=CARTESIAN_POINT('Ctrl Pts',(-15.9882020295104,8.54663071670945,1.18550557364288));
#8985=CARTESIAN_POINT('Ctrl Pts',(-16.4360812658015,8.98683941379159,1.14845852446654));
#8986=CARTESIAN_POINT('Ctrl Pts',(-16.596541603247,9.51445427072422,1.1114114752902));
#8987=CARTESIAN_POINT('Ctrl Pts',(-16.6440292858128,9.67060006501775,1.1004475290634));
#8988=CARTESIAN_POINT('Ctrl Pts',(-16.6663435686959,9.8344012716919,1.0894835828366));
#8989=CARTESIAN_POINT('Ctrl Pts',(-16.6649907195691,9.99856203207469,1.07851963660979));
#8990=CARTESIAN_POINT('Ctrl Pts',(-16.6633491135953,10.0003647770189,1.27148036339021));
#8991=CARTESIAN_POINT('Ctrl Pts',(-16.6627612147386,9.69991012970163,1.29149729167974));
#8992=CARTESIAN_POINT('Ctrl Pts',(-16.5850836111443,9.39917204021162,1.31151421996928));
#8993=CARTESIAN_POINT('Ctrl Pts',(-16.4321389673375,9.14345057537975,1.33153114825881));
#8994=CARTESIAN_POINT('Ctrl Pts',(-16.149071172998,8.67016488708435,1.36857819743515));
#8995=CARTESIAN_POINT('Ctrl Pts',(-15.6081830158149,8.3510795296454,1.40562524661149));
#8996=CARTESIAN_POINT('Ctrl Pts',(-15.0570283687243,8.33223315424277,1.44267229578783));
#8997=CARTESIAN_POINT('Ctrl Pts',(-14.5058737216337,8.31338677884013,1.47971934496417));
#8998=CARTESIAN_POINT('Ctrl Pts',(-13.9444525846355,8.59477938547379,1.51676639414051));
#8999=CARTESIAN_POINT('Ctrl Pts',(-13.6297162853131,9.04762335182059,1.55381344331685));
#9000=CARTESIAN_POINT('Ctrl Pts',(-13.3149799859908,9.5004673181674,1.59086049249319));
#9001=CARTESIAN_POINT('Ctrl Pts',(-13.2469285243443,10.1247626442273,1.62790754166953));
#9002=CARTESIAN_POINT('Ctrl Pts',(-13.4567077239444,10.634781591296,1.66495459084587));
#9003=CARTESIAN_POINT('Ctrl Pts',(-13.6664869235445,11.1448005383647,1.70200164002221));
#9004=CARTESIAN_POINT('Ctrl Pts',(-14.1540967843911,11.5405431064421,1.73904868919855));
#9005=CARTESIAN_POINT('Ctrl Pts',(-14.6963679045584,11.6408858013554,1.77609573837489));
#9006=CARTESIAN_POINT('Ctrl Pts',(-15.2386390247256,11.7412284962687,1.81314278755123));
#9007=CARTESIAN_POINT('Ctrl Pts',(-15.8355714042134,11.5461713180179,1.85018983672757));
#9008=CARTESIAN_POINT('Ctrl Pts',(-16.2139608969767,11.1449880521985,1.88723688590391));
#9009=CARTESIAN_POINT('Ctrl Pts',(-16.5007749835987,10.8408965957637,1.91531804506601));
#9010=CARTESIAN_POINT('Ctrl Pts',(-16.6620267032898,10.4183767620469,1.94339920422811));
#9011=CARTESIAN_POINT('Ctrl Pts',(-16.6658557594656,9.99847620480149,1.97148036339021));
#9012=CARTESIAN_POINT('Origin',(-15.,10.,4.));
#9013=CARTESIAN_POINT('',(-16.6685089555354,10.000563745621,2.67148036339021));
#9014=CARTESIAN_POINT('',(-16.6649202598041,10.0014222546351,2.47851963660979));
#9015=CARTESIAN_POINT('',(-16.666,10.,4.));
#9016=CARTESIAN_POINT('Ctrl Pts',(-16.6649202598041,10.0014222546351,2.47851963660979));
#9017=CARTESIAN_POINT('Ctrl Pts',(-16.6662754447434,10.1682098104616,2.46738150628601));
#9018=CARTESIAN_POINT('Ctrl Pts',(-16.6432316927311,10.3346314283879,2.45624337596222));
#9019=CARTESIAN_POINT('Ctrl Pts',(-16.5942458705854,10.4930303020904,2.44510524563844));
#9020=CARTESIAN_POINT('Ctrl Pts',(-16.431311867371,11.0198881043375,2.4080581964621));
#9021=CARTESIAN_POINT('Ctrl Pts',(-15.9813743049921,11.4579882964685,2.37101114728576));
#9022=CARTESIAN_POINT('Ctrl Pts',(-15.4503607132462,11.6068210844527,2.33396409810942));
#9023=CARTESIAN_POINT('Ctrl Pts',(-14.9193471215002,11.7556538724368,2.29691704893308));
#9024=CARTESIAN_POINT('Ctrl Pts',(-14.3072575003873,11.6152192562742,2.25986999975674));
#9025=CARTESIAN_POINT('Ctrl Pts',(-13.8942331662336,11.2497913767376,2.2228229505804));
#9026=CARTESIAN_POINT('Ctrl Pts',(-13.48120883208,10.8843634972009,2.18577590140406));
#9027=CARTESIAN_POINT('Ctrl Pts',(-13.2672497848857,10.2939423542903,2.14872885222772));
#9028=CARTESIAN_POINT('Ctrl Pts',(-13.350280857865,9.7487520471889,2.11168180305138));
#9029=CARTESIAN_POINT('Ctrl Pts',(-13.4333119308442,9.2035617400875,2.07463475387504));
#9030=CARTESIAN_POINT('Ctrl Pts',(-13.813333123997,8.70360226879533,2.0375877046987));
#9031=CARTESIAN_POINT('Ctrl Pts',(-14.3164162361929,8.4776951740808,2.00054065552236));
#9032=CARTESIAN_POINT('Ctrl Pts',(-14.8194993483888,8.25178807936627,1.96349360634602));
#9033=CARTESIAN_POINT('Ctrl Pts',(-15.4456443796278,8.2999333612294,1.92644655716968));
#9034=CARTESIAN_POINT('Ctrl Pts',(-15.9082771523615,8.60009592645602,1.88939950799334));
#9035=CARTESIAN_POINT('Ctrl Pts',(-16.3698223449295,8.8995528545734,1.85243955086549));
#9036=CARTESIAN_POINT('Ctrl Pts',(-16.668623160866,9.4498435492614,1.81547959373764));
#9037=CARTESIAN_POINT('Ctrl Pts',(-16.6687412413332,10.0000242582383,1.77851963660979));
#9038=CARTESIAN_POINT('Ctrl Pts',(-16.6658557594656,9.99847620480149,1.97148036339021));
#9039=CARTESIAN_POINT('Ctrl Pts',(-16.6670783192728,9.8644082985784,1.98044625340445));
#9040=CARTESIAN_POINT('Ctrl Pts',(-16.65225276481,9.73060740885205,1.98941214341869));
#9041=CARTESIAN_POINT('Ctrl Pts',(-16.6203420813068,9.60101349282022,1.99837803343293));
#9042=CARTESIAN_POINT('Ctrl Pts',(-16.4884871668348,9.06553155264917,2.03542508260927));
#9043=CARTESIAN_POINT('Ctrl Pts',(-16.0649307318521,8.60187702569495,2.07247213178561));
#9044=CARTESIAN_POINT('Ctrl Pts',(-15.5435261848766,8.42225541573886,2.10951918096195));
#9045=CARTESIAN_POINT('Ctrl Pts',(-15.0221216379011,8.24263380578278,2.14656623013829));
#9046=CARTESIAN_POINT('Ctrl Pts',(-14.4028689789328,8.34704511282482,2.18361327931463));
#9047=CARTESIAN_POINT('Ctrl Pts',(-13.9691879081116,8.68770234961182,2.22066032849097));
#9048=CARTESIAN_POINT('Ctrl Pts',(-13.5355068372904,9.02835958639883,2.25770737766731));
#9049=CARTESIAN_POINT('Ctrl Pts',(-13.2873973546162,9.60526275293079,2.29475442684365));
#9050=CARTESIAN_POINT('Ctrl Pts',(-13.3384142659838,10.154374671996,2.33180147601999));
#9051=CARTESIAN_POINT('Ctrl Pts',(-13.3894311773513,10.7034865910612,2.36884852519633));
#9052=CARTESIAN_POINT('Ctrl Pts',(-13.7395744827606,11.2248072626597,2.40589557437267));
#9053=CARTESIAN_POINT('Ctrl Pts',(-14.2285905127814,11.4797385218802,2.44294262354901));
#9054=CARTESIAN_POINT('Ctrl Pts',(-14.7176065428022,11.7346697811008,2.47998967272535));
#9055=CARTESIAN_POINT('Ctrl Pts',(-15.3454952974345,11.7232116279436,2.51703672190169));
#9056=CARTESIAN_POINT('Ctrl Pts',(-15.8248845058031,11.450608232057,2.55408377107803));
#9057=CARTESIAN_POINT('Ctrl Pts',(-16.3042737141718,11.1780048361704,2.59113082025437));
#9058=CARTESIAN_POINT('Ctrl Pts',(-16.6351633762768,10.6442561975546,2.62817786943071));
#9059=CARTESIAN_POINT('Ctrl Pts',(-16.66611183473,10.0936485172939,2.66522491860705));
#9060=CARTESIAN_POINT('Ctrl Pts',(-16.6678537312038,10.062658231359,2.6673100668681));
#9061=CARTESIAN_POINT('Ctrl Pts',(-16.6686454544998,10.0316145382597,2.66939521512915));
#9062=CARTESIAN_POINT('Ctrl Pts',(-16.6685089555354,10.000563745621,2.67148036339021));
#9063=CARTESIAN_POINT('Origin',(-15.,10.,4.));
#9064=CARTESIAN_POINT('',(-16.6641896231852,10.0011694308927,3.37148036339021));
#9065=CARTESIAN_POINT('',(-16.6637099363687,9.99914721740977,3.1785196366098));
#9066=CARTESIAN_POINT('',(-16.666,10.,4.));
#9067=CARTESIAN_POINT('Ctrl Pts',(-16.6637099363687,9.99914721740977,3.1785196366098));
#9068=CARTESIAN_POINT('Ctrl Pts',(-16.6621663356667,10.3320266710605,3.15633046801072));
#9069=CARTESIAN_POINT('Ctrl Pts',(-16.5654394528057,10.6657320996906,3.13414129941163));
#9070=CARTESIAN_POINT('Ctrl Pts',(-16.3796152224748,10.9388080800771,3.11195213081255));
#9071=CARTESIAN_POINT('Ctrl Pts',(-16.0693629762726,11.3947359004046,3.07490508163621));
#9072=CARTESIAN_POINT('Ctrl Pts',(-15.5107459794087,11.681655122571,3.03785803245988));
#9073=CARTESIAN_POINT('Ctrl Pts',(-14.959432188694,11.6682484904506,3.00081098328354));
#9074=CARTESIAN_POINT('Ctrl Pts',(-14.4081183979792,11.6548418583303,2.9637639341072));
#9075=CARTESIAN_POINT('Ctrl Pts',(-13.8641078134136,11.341109371923,2.92671688493086));
#9076=CARTESIAN_POINT('Ctrl Pts',(-13.5763833255364,10.8706401882922,2.88966983575452));
#9077=CARTESIAN_POINT('Ctrl Pts',(-13.2886588376591,10.4001710046614,2.85262278657818));
#9078=CARTESIAN_POINT('Ctrl Pts',(-13.2572204464702,9.77296512380708,2.81557573740183));
#9079=CARTESIAN_POINT('Ctrl Pts',(-13.4964568822746,9.27608227910361,2.77852868822549));
#9080=CARTESIAN_POINT('Ctrl Pts',(-13.7356933180791,8.77919943440014,2.74148163904915));
#9081=CARTESIAN_POINT('Ctrl Pts',(-14.2456045808769,8.41263962584757,2.70443458987282));
#9082=CARTESIAN_POINT('Ctrl Pts',(-14.7928143653133,8.34417003120825,2.66738754069648));
#9083=CARTESIAN_POINT('Ctrl Pts',(-15.3400241497496,8.27570043656892,2.63034049152014));
#9084=CARTESIAN_POINT('Ctrl Pts',(-15.9245324558244,8.50532105584284,2.5932934423438));
#9085=CARTESIAN_POINT('Ctrl Pts',(-16.278821386837,8.92793907166143,2.55624639316746));
#9086=CARTESIAN_POINT('Ctrl Pts',(-16.5265939724556,9.22349772264472,2.5303374743149));
#9087=CARTESIAN_POINT('Ctrl Pts',(-16.6617679015892,9.61345002555303,2.50442855546235));
#9088=CARTESIAN_POINT('Ctrl Pts',(-16.6649202598041,10.0014222546351,2.47851963660979));
#9089=CARTESIAN_POINT('Ctrl Pts',(-16.6685089555354,10.000563745621,2.67148036339021));
#9090=CARTESIAN_POINT('Ctrl Pts',(-16.6662202629958,9.4799318290084,2.70644226430549));
#9091=CARTESIAN_POINT('Ctrl Pts',(-16.4029750372034,8.95730397752036,2.74140416522078));
#9092=CARTESIAN_POINT('Ctrl Pts',(-15.982246261208,8.65096665241879,2.77636606613607));
#9093=CARTESIAN_POINT('Ctrl Pts',(-15.5364249744315,8.32635918971003,2.81341311531241));
#9094=CARTESIAN_POINT('Ctrl Pts',(-14.9137751460771,8.24461098619809,2.85046016448875));
#9095=CARTESIAN_POINT('Ctrl Pts',(-14.3992712940895,8.44313657871488,2.88750721366509));
#9096=CARTESIAN_POINT('Ctrl Pts',(-13.8847674421018,8.64166217123168,2.92455426284143));
#9097=CARTESIAN_POINT('Ctrl Pts',(-13.4784095664808,9.12046155977721,2.96160131201777));
#9098=CARTESIAN_POINT('Ctrl Pts',(-13.3661796340593,9.6603977290365,2.99864836119411));
#9099=CARTESIAN_POINT('Ctrl Pts',(-13.2539497016378,10.2003338982958,3.03569541037045));
#9100=CARTESIAN_POINT('Ctrl Pts',(-13.4358477124159,10.8014068482688,3.07274245954679));
#9101=CARTESIAN_POINT('Ctrl Pts',(-13.8286225426003,11.1885173717263,3.10978950872313));
#9102=CARTESIAN_POINT('Ctrl Pts',(-14.2213973727848,11.5756278951839,3.14683655789947));
#9103=CARTESIAN_POINT('Ctrl Pts',(-14.8250490223756,11.7487759921259,3.18388360707581));
#9104=CARTESIAN_POINT('Ctrl Pts',(-15.3632980642854,11.628715201347,3.22093065625215));
#9105=CARTESIAN_POINT('Ctrl Pts',(-15.9015471061952,11.5086544105681,3.25797770542849));
#9106=CARTESIAN_POINT('Ctrl Pts',(-16.374393540424,11.0953847320682,3.29502475460482));
#9107=CARTESIAN_POINT('Ctrl Pts',(-16.5654249012081,10.5780515282261,3.33207180378116));
#9108=CARTESIAN_POINT('Ctrl Pts',(-16.6331610271708,10.3946149086246,3.34520799031751));
#9109=CARTESIAN_POINT('Ctrl Pts',(-16.6654651595513,10.1980946093002,3.35834417685386));
#9110=CARTESIAN_POINT('Ctrl Pts',(-16.6641896231852,10.0011694308927,3.37148036339021));
#9111=CARTESIAN_POINT('Origin',(-15.,10.,4.));
#9112=CARTESIAN_POINT('',(-16.6642806308315,9.99878755139411,4.07148036339021));
#9113=CARTESIAN_POINT('',(-16.6680322603961,9.99903395438687,3.8785196366098));
#9114=CARTESIAN_POINT('',(-16.666,10.,4.));
#9115=CARTESIAN_POINT('Ctrl Pts',(-16.6680322603961,9.99903395438687,3.8785196366098));
#9116=CARTESIAN_POINT('Ctrl Pts',(-16.6646131543622,10.494401776487,3.84527942973542));
#9117=CARTESIAN_POINT('Ctrl Pts',(-16.4297940317408,10.9925842260247,3.81203922286105));
#9118=CARTESIAN_POINT('Ctrl Pts',(-16.043711877959,11.3020615534902,3.77879901598667));
#9119=CARTESIAN_POINT('Ctrl Pts',(-15.6134135771296,11.6469818427323,3.74175196681033));
#9120=CARTESIAN_POINT('Ctrl Pts',(-14.995221408434,11.7574989536148,3.70470491763399));
#9121=CARTESIAN_POINT('Ctrl Pts',(-14.4720697071203,11.5830313891797,3.66765786845765));
#9122=CARTESIAN_POINT('Ctrl Pts',(-13.9489180058066,11.4085638247447,3.63061081928131));
#9123=CARTESIAN_POINT('Ctrl Pts',(-13.5208067718749,10.9491115849921,3.59356377010497));
#9124=CARTESIAN_POINT('Ctrl Pts',(-13.3836740542319,10.4149568776457,3.55651672092864));
#9125=CARTESIAN_POINT('Ctrl Pts',(-13.2465413365889,9.88080217029943,3.5194696717523));
#9126=CARTESIAN_POINT('Ctrl Pts',(-13.4003871352347,9.27194499535936,3.48242262257596));
#9127=CARTESIAN_POINT('Ctrl Pts',(-13.7747992693407,8.86704724596919,3.44537557339962));
#9128=CARTESIAN_POINT('Ctrl Pts',(-14.1492114034467,8.46214949657901,3.40832852422328));
#9129=CARTESIAN_POINT('Ctrl Pts',(-14.744189873013,8.26121117273875,3.37128147504693));
#9130=CARTESIAN_POINT('Ctrl Pts',(-15.2874247939926,8.35619777313096,3.3342344258706));
#9131=CARTESIAN_POINT('Ctrl Pts',(-15.8306597149722,8.45118437352318,3.29718737669425));
#9132=CARTESIAN_POINT('Ctrl Pts',(-16.3221510873651,8.84209589814789,3.26014032751792));
#9133=CARTESIAN_POINT('Ctrl Pts',(-16.5369530257913,9.3500198697045,3.22309327834158));
#9134=CARTESIAN_POINT('Ctrl Pts',(-16.6231002796173,9.55372499277096,3.20823539776432));
#9135=CARTESIAN_POINT('Ctrl Pts',(-16.6647435323228,9.77625093597039,3.19337751718706));
#9136=CARTESIAN_POINT('Ctrl Pts',(-16.6637099363687,9.99914721740977,3.1785196366098));
#9137=CARTESIAN_POINT('Ctrl Pts',(-16.6641896231852,10.0011694308927,3.37148036339021));
#9138=CARTESIAN_POINT('Ctrl Pts',(-16.6618678553907,9.64272058592326,3.3953912260302));
#9139=CARTESIAN_POINT('Ctrl Pts',(-16.5482888473394,9.28293028253278,3.4193020886702));
#9140=CARTESIAN_POINT('Ctrl Pts',(-16.3346236739081,8.99826233990597,3.44321295131019));
#9141=CARTESIAN_POINT('Ctrl Pts',(-16.0035747984843,8.55720308461235,3.48026000048653));
#9142=CARTESIAN_POINT('Ctrl Pts',(-15.4322607602971,8.2964813032095,3.51730704966287));
#9143=CARTESIAN_POINT('Ctrl Pts',(-14.8821607009425,8.33542420112334,3.5543540988392));
#9144=CARTESIAN_POINT('Ctrl Pts',(-14.332060641588,8.37436709903719,3.59140114801554));
#9145=CARTESIAN_POINT('Ctrl Pts',(-13.8031745610662,8.71297467626774,3.62844819719189));
#9146=CARTESIAN_POINT('Ctrl Pts',(-13.5375631634618,9.19627293827846,3.66549524636823));
#9147=CARTESIAN_POINT('Ctrl Pts',(-13.2719517658575,9.67957120028917,3.70254229554457));
#9148=CARTESIAN_POINT('Ctrl Pts',(-13.2696150511706,10.30756014708,3.73958934472091));
#9149=CARTESIAN_POINT('Ctrl Pts',(-13.5316224875214,10.7928216517316,3.77663639389725));
#9150=CARTESIAN_POINT('Ctrl Pts',(-13.7936299238721,11.2780831563831,3.81368344307358));
#9151=CARTESIAN_POINT('Ctrl Pts',(-14.3199815112606,11.6206172188953,3.85073049224993));
#9152=CARTESIAN_POINT('Ctrl Pts',(-14.8697765330075,11.6636527700371,3.88777754142627));
#9153=CARTESIAN_POINT('Ctrl Pts',(-15.4195715547545,11.7066883211789,3.92482459060261));
#9154=CARTESIAN_POINT('Ctrl Pts',(-15.99281001086,11.4502253609502,3.96187163977895));
#9155=CARTESIAN_POINT('Ctrl Pts',(-16.3271319916882,11.0116419165125,3.99891868895529));
#9156=CARTESIAN_POINT('Ctrl Pts',(-16.5454036513628,10.7253001806623,4.02310591376693));
#9157=CARTESIAN_POINT('Ctrl Pts',(-16.6618370586765,10.3613295085513,4.04729313857857));
#9158=CARTESIAN_POINT('Ctrl Pts',(-16.6642806308315,9.99878755139411,4.07148036339021));
#9159=CARTESIAN_POINT('Origin',(-15.,10.,4.));
#9160=CARTESIAN_POINT('',(-16.6685641298519,9.99950756874516,4.77148036339021));
#9161=CARTESIAN_POINT('',(-16.66663599516,10.0014616028905,4.5785196366098));
#9162=CARTESIAN_POINT('',(-16.666,10.,4.));
#9163=CARTESIAN_POINT('Ctrl Pts',(-16.66663599516,10.0014616028905,4.5785196366098));
#9164=CARTESIAN_POINT('Ctrl Pts',(-16.6676283665625,10.1096548573022,4.57127544063647));
#9165=CARTESIAN_POINT('Ctrl Pts',(-16.6579946337124,10.2176721666637,4.56403124466314));
#9166=CARTESIAN_POINT('Ctrl Pts',(-16.6370920864311,10.323462940401,4.55678704868981));
#9167=CARTESIAN_POINT('Ctrl Pts',(-16.5301957931928,10.8644803302501,4.51973999951347));
#9168=CARTESIAN_POINT('Ctrl Pts',(-16.1285825664142,11.3472664167428,4.48269295033713));
#9169=CARTESIAN_POINT('Ctrl Pts',(-15.6160628409387,11.5508595517598,4.44564590116079));
#9170=CARTESIAN_POINT('Ctrl Pts',(-15.1035431154632,11.7544526867768,4.40859885198445));
#9171=CARTESIAN_POINT('Ctrl Pts',(-14.4801168912907,11.6788528703182,4.37155180280811));
#9172=CARTESIAN_POINT('Ctrl Pts',(-14.0311140273948,11.3586606439277,4.33450475363177));
#9173=CARTESIAN_POINT('Ctrl Pts',(-13.5821111634988,11.0384684175371,4.29745770445543));
#9174=CARTESIAN_POINT('Ctrl Pts',(-13.3075316598793,10.4736837812147,4.26041065527909));
#9175=CARTESIAN_POINT('Ctrl Pts',(-13.3330451274809,9.92279749839539,4.22336360610275));
#9176=CARTESIAN_POINT('Ctrl Pts',(-13.3585585950825,9.37191121557606,4.18631655692641));
#9177=CARTESIAN_POINT('Ctrl Pts',(-13.6841650339053,8.83492328625981,4.14926950775007));
#9178=CARTESIAN_POINT('Ctrl Pts',(-14.1608408134576,8.55760247056822,4.11222245857373));
#9179=CARTESIAN_POINT('Ctrl Pts',(-14.6375165930098,8.28028165487663,4.07517540939739));
#9180=CARTESIAN_POINT('Ctrl Pts',(-15.2652617132915,8.2626279528097,4.03812836022105));
#9181=CARTESIAN_POINT('Ctrl Pts',(-15.756769641956,8.51272111482649,4.00108131104471));
#9182=CARTESIAN_POINT('Ctrl Pts',(-16.2482775706204,8.76281427684328,3.96403426186837));
#9183=CARTESIAN_POINT('Ctrl Pts',(-16.6035483076676,9.28065430294379,3.92698721269203));
#9184=CARTESIAN_POINT('Ctrl Pts',(-16.6599814597096,9.82923604979498,3.88994016351569));
#9185=CARTESIAN_POINT('Ctrl Pts',(-16.6657803590876,9.88560664465826,3.88613332121373));
#9186=CARTESIAN_POINT('Ctrl Pts',(-16.6684238342973,9.94230184115634,3.88232647891176));
#9187=CARTESIAN_POINT('Ctrl Pts',(-16.6680322603961,9.99903395438687,3.8785196366098));
#9188=CARTESIAN_POINT('Ctrl Pts',(-16.6642806308315,9.99878755139411,4.07148036339021));
#9189=CARTESIAN_POINT('Ctrl Pts',(-16.6655798253021,9.80603183302699,4.08434018775491));
#9190=CARTESIAN_POINT('Ctrl Pts',(-16.6346561573177,9.61367998650847,4.09720001211961));
#9191=CARTESIAN_POINT('Ctrl Pts',(-16.5696832944175,9.43361404869653,4.11005983648431));
#9192=CARTESIAN_POINT('Ctrl Pts',(-16.3825071107676,8.91487355396514,4.14710688566065));
#9193=CARTESIAN_POINT('Ctrl Pts',(-15.9127492379168,8.49809649314917,4.18415393483699));
#9194=CARTESIAN_POINT('Ctrl Pts',(-15.3754085681396,8.37403348817524,4.22120098401333));
#9195=CARTESIAN_POINT('Ctrl Pts',(-14.8380678983624,8.24997048320131,4.25824803318967));
#9196=CARTESIAN_POINT('Ctrl Pts',(-14.2331444316588,8.41862153406943,4.295295082366));
#9197=CARTESIAN_POINT('Ctrl Pts',(-13.837499680669,8.80279838867386,4.33234213154234));
#9198=CARTESIAN_POINT('Ctrl Pts',(-13.4418549296792,9.18697524327829,4.36938918071868));
#9199=CARTESIAN_POINT('Ctrl Pts',(-13.2554888944033,9.78667790161905,4.40643622989502));
#9200=CARTESIAN_POINT('Ctrl Pts',(-13.3636976251207,10.3274343118419,4.44348327907136));
#9201=CARTESIAN_POINT('Ctrl Pts',(-13.4719063558382,10.8681907220648,4.4805303282477));
#9202=CARTESIAN_POINT('Ctrl Pts',(-13.874689852549,11.3500008841698,4.51757737742404));
#9203=CARTESIAN_POINT('Ctrl Pts',(-14.3877020709949,11.5523498113339,4.55462442660038));
#9204=CARTESIAN_POINT('Ctrl Pts',(-14.9007142894408,11.754698738498,4.59167147577672));
#9205=CARTESIAN_POINT('Ctrl Pts',(-15.5239552296219,11.6775864307212,4.62871852495307));
#9206=CARTESIAN_POINT('Ctrl Pts',(-15.9721798333851,11.3563056669346,4.6657655741294));
#9207=CARTESIAN_POINT('Ctrl Pts',(-16.3985203074742,11.050711123488,4.70100383721634));
#9208=CARTESIAN_POINT('Ctrl Pts',(-16.666517248032,10.5242086528571,4.73624210030327));
#9209=CARTESIAN_POINT('Ctrl Pts',(-16.6685641298519,9.99950756874516,4.77148036339021));
#9210=CARTESIAN_POINT('Origin',(-15.,10.,4.));
#9211=CARTESIAN_POINT('',(-16.665731796286,10.0015218067206,5.47148036339021));
#9212=CARTESIAN_POINT('',(-16.6632774972289,10.0000562476522,5.2785196366098));
#9213=CARTESIAN_POINT('',(-16.666,10.,4.));
#9214=CARTESIAN_POINT('Ctrl Pts',(-16.6632774972289,10.0000562476522,5.2785196366098));
#9215=CARTESIAN_POINT('Ctrl Pts',(-16.6633601998516,10.2746976550433,5.26022440236118));
#9216=CARTESIAN_POINT('Ctrl Pts',(-16.5991042841727,10.5493026373111,5.24192916811255));
#9217=CARTESIAN_POINT('Ctrl Pts',(-16.4702969568271,10.7892563791,5.22363393386393));
#9218=CARTESIAN_POINT('Ctrl Pts',(-16.2094677525875,11.2751522113859,5.1865868846876));
#9219=CARTESIAN_POINT('Ctrl Pts',(-15.6839488500416,11.6189624385472,5.14953983551125));
#9220=CARTESIAN_POINT('Ctrl Pts',(-15.1342598624345,11.663331915957,5.11249278633491));
#9221=CARTESIAN_POINT('Ctrl Pts',(-14.5845708748275,11.7077013933668,5.07544573715857));
#9222=CARTESIAN_POINT('Ctrl Pts',(-14.0107118021594,11.4526301210251,5.03839868798223));
#9223=CARTESIAN_POINT('Ctrl Pts',(-13.67532659802,11.0148591780905,5.00135163880589));
#9224=CARTESIAN_POINT('Ctrl Pts',(-13.3399413938806,10.5770882351559,4.96430458962955));
#9225=CARTESIAN_POINT('Ctrl Pts',(-13.2430300582699,9.95661762162842,4.92725754045321));
#9226=CARTESIAN_POINT('Ctrl Pts',(-13.4289469937516,9.43742447189813,4.89021049127687));
#9227=CARTESIAN_POINT('Ctrl Pts',(-13.6148639292333,8.91823132216784,4.85316344210053));
#9228=CARTESIAN_POINT('Ctrl Pts',(-14.0836091358075,8.50031563623478,4.81611639292419));
#9229=CARTESIAN_POINT('Ctrl Pts',(-14.6206471985419,8.37494916224136,4.77906934374785));
#9230=CARTESIAN_POINT('Ctrl Pts',(-15.1576852612763,8.24958268824794,4.74202229457151));
#9231=CARTESIAN_POINT('Ctrl Pts',(-15.7630161801709,8.41676542619417,4.70497524539517));
#9232=CARTESIAN_POINT('Ctrl Pts',(-16.1595919597692,8.79998114177013,4.66792819621883));
#9233=CARTESIAN_POINT('Ctrl Pts',(-16.4786211403925,9.10826269105184,4.63812534301582));
#9234=CARTESIAN_POINT('Ctrl Pts',(-16.6625533475701,9.55635110468484,4.60832248981281));
#9235=CARTESIAN_POINT('Ctrl Pts',(-16.66663599516,10.0014616028905,4.5785196366098));
#9236=CARTESIAN_POINT('Ctrl Pts',(-16.6685641298519,9.99950756874516,4.77148036339021));
#9237=CARTESIAN_POINT('Ctrl Pts',(-16.6686691966469,9.9725745720848,4.77328914947961));
#9238=CARTESIAN_POINT('Ctrl Pts',(-16.6680735418144,9.94564632169335,4.77509793556902));
#9239=CARTESIAN_POINT('Ctrl Pts',(-16.6667626122128,9.91875293767893,4.77690672165842));
#9240=CARTESIAN_POINT('Ctrl Pts',(-16.639912519932,9.36793019200639,4.81395377083476));
#9241=CARTESIAN_POINT('Ctrl Pts',(-16.313004068025,8.83173392045779,4.8510008200111));
#9242=CARTESIAN_POINT('Ctrl Pts',(-15.8356567926335,8.55557055708282,4.88804786918744));
#9243=CARTESIAN_POINT('Ctrl Pts',(-15.358309517242,8.27940719370785,4.92509491836379));
#9244=CARTESIAN_POINT('Ctrl Pts',(-14.7305234183659,8.2632767385065,4.96214196754013));
#9245=CARTESIAN_POINT('Ctrl Pts',(-14.239623783446,8.51456178188315,4.99918901671647));
#9246=CARTESIAN_POINT('Ctrl Pts',(-13.7487241485261,8.76584682525981,5.03623606589281));
#9247=CARTESIAN_POINT('Ctrl Pts',(-13.3947109775624,9.28454736721446,5.07328311506914));
#9248=CARTESIAN_POINT('Ctrl Pts',(-13.339609100803,9.83326442346505,5.11033016424548));
#9249=CARTESIAN_POINT('Ctrl Pts',(-13.2845072240436,10.3819814797156,5.14737721342182));
#9250=CARTESIAN_POINT('Ctrl Pts',(-13.5283166414883,10.9607150502622,5.18442426259816));
#9251=CARTESIAN_POINT('Ctrl Pts',(-13.9594506023805,11.3045902199309,5.2214713117745));
#9252=CARTESIAN_POINT('Ctrl Pts',(-14.3905845632726,11.6484653895996,5.25851836095084));
#9253=CARTESIAN_POINT('Ctrl Pts',(-15.009043067612,11.7574821583904,5.29556541012718));
#9254=CARTESIAN_POINT('Ctrl Pts',(-15.5317698835803,11.5817457068139,5.33261245930352));
#9255=CARTESIAN_POINT('Ctrl Pts',(-16.0544966995486,11.4060092552373,5.36965950847986));
#9256=CARTESIAN_POINT('Ctrl Pts',(-16.4814918271458,10.9455195832933,5.4067065576562));
#9257=CARTESIAN_POINT('Ctrl Pts',(-16.6173280372926,10.411033709843,5.44375360683254));
#9258=CARTESIAN_POINT('Ctrl Pts',(-16.6512155543302,10.2776937180744,5.45299585901843));
#9259=CARTESIAN_POINT('Ctrl Pts',(-16.6669822248687,10.1397484275201,5.46223811120432));
#9260=CARTESIAN_POINT('Ctrl Pts',(-16.665731796286,10.0015218067206,5.47148036339021));
#9261=CARTESIAN_POINT('Origin',(-15.,10.,4.));
#9262=CARTESIAN_POINT('',(-16.6633786660592,9.9995695770803,6.17148036339021));
#9263=CARTESIAN_POINT('',(-16.6664295062294,9.99850933107572,5.9785196366098));
#9264=CARTESIAN_POINT('',(-16.666,10.,4.));
#9265=CARTESIAN_POINT('Ctrl Pts',(-16.6664295062294,9.99850933107572,5.9785196366098));
#9266=CARTESIAN_POINT('Ctrl Pts',(-16.6623835386158,10.4369404484093,5.94917336408588));
#9267=CARTESIAN_POINT('Ctrl Pts',(-16.4846437176932,10.8782736700321,5.91982709156197));
#9268=CARTESIAN_POINT('Ctrl Pts',(-16.1742579084843,11.1856715961173,5.89048081903805));
#9269=CARTESIAN_POINT('Ctrl Pts',(-15.7824235340154,11.5737340348854,5.85343376986171));
#9270=CARTESIAN_POINT('Ctrl Pts',(-15.1791937896595,11.7483463595048,5.81638672068537));
#9271=CARTESIAN_POINT('Ctrl Pts',(-14.6406550026031,11.6295919573634,5.77933967150903));
#9272=CARTESIAN_POINT('Ctrl Pts',(-14.1021162155467,11.5108375552221,5.74229262233269));
#9273=CARTESIAN_POINT('Ctrl Pts',(-13.6282683857898,11.09871642632,5.70524557315635));
#9274=CARTESIAN_POINT('Ctrl Pts',(-13.4359822991767,10.5818482663145,5.66819852398002));
#9275=CARTESIAN_POINT('Ctrl Pts',(-13.2436962125636,10.064980106309,5.63115147480367));
#9276=CARTESIAN_POINT('Ctrl Pts',(-13.3329718690941,9.44336491520019,5.59410442562733));
#9277=CARTESIAN_POINT('Ctrl Pts',(-13.662949564977,9.00150367703514,5.55705737645099));
#9278=CARTESIAN_POINT('Ctrl Pts',(-13.9929272608599,8.55964243887008,5.52001032727465));
#9279=CARTESIAN_POINT('Ctrl Pts',(-14.5636069960951,8.29753515364879,5.48296327809831));
#9280=CARTESIAN_POINT('Ctrl Pts',(-15.1137999373131,8.33514314496572,5.44591622892197));
#9281=CARTESIAN_POINT('Ctrl Pts',(-15.6639928785312,8.37275113628264,5.40886917974563));
#9282=CARTESIAN_POINT('Ctrl Pts',(-16.193699025732,8.71007440413778,5.37182213056929));
#9283=CARTESIAN_POINT('Ctrl Pts',(-16.4604823463659,9.19272675677063,5.33477508139295));
#9284=CARTESIAN_POINT('Ctrl Pts',(-16.5955179717545,9.43702712055721,5.31602326646523));
#9285=CARTESIAN_POINT('Ctrl Pts',(-16.6631927306577,9.71856081704436,5.29727145153751));
#9286=CARTESIAN_POINT('Ctrl Pts',(-16.6632774972289,10.0000562476522,5.2785196366098));
#9287=CARTESIAN_POINT('Ctrl Pts',(-16.665731796286,10.0015218067206,5.47148036339021));
#9288=CARTESIAN_POINT('Ctrl Pts',(-16.6619699520738,9.58567477585555,5.49928516038066));
#9289=CARTESIAN_POINT('Ctrl Pts',(-16.504190860803,9.16728149961843,5.52708995737111));
#9290=CARTESIAN_POINT('Ctrl Pts',(-16.2224480480665,8.86407770434065,5.55489475436156));
#9291=CARTESIAN_POINT('Ctrl Pts',(-15.847054555997,8.46008964724508,5.5919418035379));
#9292=CARTESIAN_POINT('Ctrl Pts',(-15.2515902791614,8.26059560801048,5.62898885271424));
#9293=CARTESIAN_POINT('Ctrl Pts',(-14.7085874460709,8.3569000607923,5.66603590189058));
#9294=CARTESIAN_POINT('Ctrl Pts',(-14.1655846129804,8.45320451357413,5.70308295106692));
#9295=CARTESIAN_POINT('Ctrl Pts',(-13.6750432236349,8.84530745837239,5.74013000024326));
#9296=CARTESIAN_POINT('Ctrl Pts',(-13.461474374797,9.35375113620292,5.7771770494196));
#9297=CARTESIAN_POINT('Ctrl Pts',(-13.2479055259592,9.86219481403344,5.81422409859594));
#9298=CARTESIAN_POINT('Ctrl Pts',(-13.3113092176289,10.4869792248962,5.85127114777228));
#9299=CARTESIAN_POINT('Ctrl Pts',(-13.6226668338069,10.9421528795107,5.88831819694862));
#9300=CARTESIAN_POINT('Ctrl Pts',(-13.9340244499849,11.3973265341252,5.92536524612496));
#9301=CARTESIAN_POINT('Ctrl Pts',(-14.4933359906712,11.6828894324913,5.9624122953013));
#9302=CARTESIAN_POINT('Ctrl Pts',(-15.0446156194918,11.6681451102855,5.99945934447764));
#9303=CARTESIAN_POINT('Ctrl Pts',(-15.5958952483124,11.6534007880796,6.03650639365398));
#9304=CARTESIAN_POINT('Ctrl Pts',(-16.1391429652673,11.3383492453018,6.07355344283032));
#9305=CARTESIAN_POINT('Ctrl Pts',(-16.4257250303767,10.8671832884336,6.11060049200666));
#9306=CARTESIAN_POINT('Ctrl Pts',(-16.5827063073618,10.6090923518887,6.13089378246784));
#9307=CARTESIAN_POINT('Ctrl Pts',(-16.6626743340805,10.304158846593,6.15118707292903));
#9308=CARTESIAN_POINT('Ctrl Pts',(-16.6633786660592,9.9995695770803,6.17148036339021));
#9309=CARTESIAN_POINT('Origin',(-15.,10.,4.));
#9310=CARTESIAN_POINT('',(-16.6673099161007,9.99870037981829,6.87148036339021));
#9311=CARTESIAN_POINT('',(-16.6681787596498,10.0008675363463,6.67851963660979));
#9312=CARTESIAN_POINT('',(-16.666,10.,4.));
#9313=CARTESIAN_POINT('Ctrl Pts',(-16.6681787596498,10.0008675363463,6.67851963660979));
#9314=CARTESIAN_POINT('Ctrl Pts',(-16.6684948606872,10.0507838420897,6.67516937498693));
#9315=CARTESIAN_POINT('Ctrl Pts',(-16.6664485977206,10.1006738719505,6.67181911336406));
#9316=CARTESIAN_POINT('Ctrl Pts',(-16.6619555158093,10.1503425574736,6.66846885174119));
#9317=CARTESIAN_POINT('Ctrl Pts',(-16.6122712089522,10.6995767493754,6.63142180256485));
#9318=CARTESIAN_POINT('Ctrl Pts',(-16.2633937611776,11.2217453066089,6.59437475338851));
#9319=CARTESIAN_POINT('Ctrl Pts',(-15.7749977113418,11.4778623470653,6.55732770421217));
#9320=CARTESIAN_POINT('Ctrl Pts',(-15.286601661506,11.7339793875217,6.52028065503583));
#9321=CARTESIAN_POINT('Ctrl Pts',(-14.658687009609,11.724044911201,6.48323360585949));
#9322=CARTESIAN_POINT('Ctrl Pts',(-14.178637761833,11.4526055538444,6.44618655668315));
#9323=CARTESIAN_POINT('Ctrl Pts',(-13.6985885140571,11.1811661964878,6.40913950750681));
#9324=CARTESIAN_POINT('Ctrl Pts',(-13.3664046704023,10.6482219580952,6.37209245833047));
#9325=CARTESIAN_POINT('Ctrl Pts',(-13.3341202701254,10.0976909730731,6.33504540915413));
#9326=CARTESIAN_POINT('Ctrl Pts',(-13.3018358698486,9.54715998805105,6.29799835997779));
#9327=CARTESIAN_POINT('Ctrl Pts',(-13.5694509129499,8.97904225639946,6.26095131080145));
#9328=CARTESIAN_POINT('Ctrl Pts',(-14.0144832531239,8.65335398608828,6.22390426162511));
#9329=CARTESIAN_POINT('Ctrl Pts',(-14.459515593298,8.3276657157771,6.18685721244877));
#9330=CARTESIAN_POINT('Ctrl Pts',(-15.0819652305448,8.24440690680633,6.14981016327243));
#9331=CARTESIAN_POINT('Ctrl Pts',(-15.5969492865558,8.44168349460096,6.11276311409609));
#9332=CARTESIAN_POINT('Ctrl Pts',(-16.1119333425668,8.63896008239559,6.07571606491975));
#9333=CARTESIAN_POINT('Ctrl Pts',(-16.5194518173418,9.11677206695562,6.03866901574341));
#9334=CARTESIAN_POINT('Ctrl Pts',(-16.6329915524384,9.65643433569403,6.00162196656707));
#9335=CARTESIAN_POINT('Ctrl Pts',(-16.6565924642679,9.76861111337784,5.99392118991465));
#9336=CARTESIAN_POINT('Ctrl Pts',(-16.6674912115247,9.8834603036632,5.98622041326222));
#9337=CARTESIAN_POINT('Ctrl Pts',(-16.6664295062294,9.99850933107572,5.9785196366098));
#9338=CARTESIAN_POINT('Ctrl Pts',(-16.6633786660592,9.9995695770803,6.17148036339021));
#9339=CARTESIAN_POINT('Ctrl Pts',(-16.6639601492863,9.7481064080884,6.18823412210537));
#9340=CARTESIAN_POINT('Ctrl Pts',(-16.6105167436314,9.49687786479725,6.20498788082053));
#9341=CARTESIAN_POINT('Ctrl Pts',(-16.5017821168752,9.27243611128139,6.22174163953568));
#9342=CARTESIAN_POINT('Ctrl Pts',(-16.2613407250004,8.77613526195597,6.25878868871202));
#9343=CARTESIAN_POINT('Ctrl Pts',(-15.7505415279869,8.41081393426368,6.29583573788836));
#9344=CARTESIAN_POINT('Ctrl Pts',(-15.2031672253873,8.34367226516766,6.3328827870647));
#9345=CARTESIAN_POINT('Ctrl Pts',(-14.6557929227877,8.27653059607164,6.36992983624104));
#9346=CARTESIAN_POINT('Ctrl Pts',(-14.0718435146019,8.50756858557189,6.40697688541738));
#9347=CARTESIAN_POINT('Ctrl Pts',(-13.7185810927601,8.93104512595157,6.44402393459372));
#9348=CARTESIAN_POINT('Ctrl Pts',(-13.3653186709184,9.35452166633125,6.48107098377006));
#9349=CARTESIAN_POINT('Ctrl Pts',(-13.2427432354206,9.97043675759037,6.5181180329464));
#9350=CARTESIAN_POINT('Ctrl Pts',(-13.4069551569713,10.4968974375652,6.55516508212274));
#9351=CARTESIAN_POINT('Ctrl Pts',(-13.571167078522,11.0233581175401,6.59221213129908));
#9352=CARTESIAN_POINT('Ctrl Pts',(-14.0221663571212,11.4603643862307,6.62925918047542));
#9353=CARTESIAN_POINT('Ctrl Pts',(-14.553539505443,11.6079086639697,6.66630622965176));
#9354=CARTESIAN_POINT('Ctrl Pts',(-15.0849126537649,11.7554529417086,6.7033532788281));
#9355=CARTESIAN_POINT('Ctrl Pts',(-15.6966596718095,11.6135352284959,6.74040032800444));
#9356=CARTESIAN_POINT('Ctrl Pts',(-16.1087961059817,11.247105450898,6.77744737718078));
#9357=CARTESIAN_POINT('Ctrl Pts',(-16.4574916205823,10.9370808831329,6.80879170591726));
#9358=CARTESIAN_POINT('Ctrl Pts',(-16.6632996251162,10.4663435453455,6.84013603465373));
#9359=CARTESIAN_POINT('Ctrl Pts',(-16.6673099161007,9.99870037981829,6.87148036339021));
#9360=CARTESIAN_POINT('Origin',(-15.,10.,4.));
#9361=CARTESIAN_POINT('',(-16.6674569633666,10.0012065537184,7.57148036339021));
#9362=CARTESIAN_POINT('',(-16.6638185641669,10.0009395545784,7.3785196366098));
#9363=CARTESIAN_POINT('',(-16.666,10.,4.));
#9364=CARTESIAN_POINT('',(-13.7309291201476,11.0793586530485,8.));
#9365=CARTESIAN_POINT('Ctrl Pts',(-16.6674569633666,10.0012065537184,7.57148036339021));
#9366=CARTESIAN_POINT('Ctrl Pts',(-16.6635088351118,9.52850380962102,7.60317909473112));
#9367=CARTESIAN_POINT('Ctrl Pts',(-16.4524516198717,9.05282917058819,7.63487782607203));
#9368=CARTESIAN_POINT('Ctrl Pts',(-16.0968413167821,8.74254092877981,7.66657655741294));
#9369=CARTESIAN_POINT('Ctrl Pts',(-15.6812312330697,8.37989979877725,7.70362360658928));
#9370=CARTESIAN_POINT('Ctrl Pts',(-15.0681740060149,8.24316232925988,7.74067065576562));
#9371=CARTESIAN_POINT('Ctrl Pts',(-14.5382155648778,8.39611193633351,7.77771770494196));
#9372=CARTESIAN_POINT('Ctrl Pts',(-14.0082571237407,8.54906154340714,7.8147647541183));
#9373=CARTESIAN_POINT('Ctrl Pts',(-13.5613974685214,8.99169822707177,7.85181180329464));
#9374=CARTESIAN_POINT('Ctrl Pts',(-13.4023347302998,9.51877034776798,7.88885885247098));
#9375=CARTESIAN_POINT('Ctrl Pts',(-13.2432719920782,10.0458424684642,7.92590590164732));
#9376=CARTESIAN_POINT('Ctrl Pts',(-13.3720061708544,10.657350026192,7.96295295082366));
#9377=CARTESIAN_POINT('Ctrl Pts',(-13.7309291201476,11.0793586530485,8.));
#9378=CARTESIAN_POINT('',(-16.2714529275337,11.0812362047421,8.));
#9379=CARTESIAN_POINT('Origin',(-15.,10.,8.));
#9380=CARTESIAN_POINT('Ctrl Pts',(-16.271453753893,11.081236856086,8.));
#9381=CARTESIAN_POINT('Ctrl Pts',(-15.920559526648,11.4928281424795,7.96367382485347));
#9382=CARTESIAN_POINT('Ctrl Pts',(-15.3505267893051,11.7187789801255,7.92734764970694));
#9383=CARTESIAN_POINT('Ctrl Pts',(-14.8130932173799,11.6581104500235,7.89102147456041));
#9384=CARTESIAN_POINT('Ctrl Pts',(-14.2649945560753,11.5962379845332,7.85397442538407));
#9385=CARTESIAN_POINT('Ctrl Pts',(-13.7508017247742,11.2362576554198,7.81692737620773));
#9386=CARTESIAN_POINT('Ctrl Pts',(-13.5055196558539,10.7424222226956,7.77988032703139));
#9387=CARTESIAN_POINT('Ctrl Pts',(-13.2602375869336,10.2485867899714,7.74283327785505));
#9388=CARTESIAN_POINT('Ctrl Pts',(-13.2838662803941,9.62089625363646,7.70578622867871));
#9389=CARTESIAN_POINT('Ctrl Pts',(-13.5657615787267,9.14688997129425,7.66873917950237));
#9390=CARTESIAN_POINT('Ctrl Pts',(-13.8476568770592,8.67288368895204,7.63169213032603));
#9391=CARTESIAN_POINT('Ctrl Pts',(-14.3878187802639,8.35256166060256,7.59464508114969));
#9392=CARTESIAN_POINT('Ctrl Pts',(-14.9389380812345,8.3323961008681,7.55759803197335));
#9393=CARTESIAN_POINT('Ctrl Pts',(-15.490057382205,8.31223054113365,7.52055098279701));
#9394=CARTESIAN_POINT('Ctrl Pts',(-16.0521340809416,8.59222145001422,7.48350393362067));
#9395=CARTESIAN_POINT('Ctrl Pts',(-16.3679620729449,9.04429105270523,7.44645688444433));
#9396=CARTESIAN_POINT('Ctrl Pts',(-16.5610182455944,9.32062763298445,7.42381113516615));
#9397=CARTESIAN_POINT('Ctrl Pts',(-16.6620633433819,9.66126158882507,7.40116538588798));
#9398=CARTESIAN_POINT('Ctrl Pts',(-16.6638185641669,10.0009395545784,7.3785196366098));
#9399=CARTESIAN_POINT('Origin',(-15.,-10.,4.));
#9400=CARTESIAN_POINT('',(-16.6671910371619,-9.99865073764983,0.571480363390209));
#9401=CARTESIAN_POINT('',(-16.6635932794994,-9.99933537909448,0.378519636609792));
#9402=CARTESIAN_POINT('',(-16.666,-10.,4.));
#9403=CARTESIAN_POINT('',(-13.3882904778579,-10.4218393251423,0.));
#9404=CARTESIAN_POINT('Ctrl Pts',(-16.6635932794994,-9.99933537909448,0.378519636609792));
#9405=CARTESIAN_POINT('Ctrl Pts',(-16.6645714516563,-9.77385592384011,0.363487571935548));
#9406=CARTESIAN_POINT('Ctrl Pts',(-16.6219039270364,-9.54871059169984,0.348455507261303));
#9407=CARTESIAN_POINT('Ctrl Pts',(-16.5338111352405,-9.34297002313031,0.333423442587059));
#9408=CARTESIAN_POINT('Ctrl Pts',(-16.3167033685785,-8.83591519556408,0.29637639341072));
#9409=CARTESIAN_POINT('Ctrl Pts',(-15.8236855882005,-8.44672359513559,0.25932934423438));
#9410=CARTESIAN_POINT('Ctrl Pts',(-15.2798473371766,-8.35458603397586,0.222282295058041));
#9411=CARTESIAN_POINT('Ctrl Pts',(-14.7360090861527,-8.26244847281612,0.185235245881701));
#9412=CARTESIAN_POINT('Ctrl Pts',(-14.1413503644829,-8.46736495092516,0.14818819670536));
#9413=CARTESIAN_POINT('Ctrl Pts',(-13.7693517818271,-8.87322579748708,0.111141147529019));
#9414=CARTESIAN_POINT('Ctrl Pts',(-13.3973531991712,-9.279086644049,0.0740940983526794));
#9415=CARTESIAN_POINT('Ctrl Pts',(-13.2480147555294,-9.88589185906381,0.0370470491763398));
#9416=CARTESIAN_POINT('Ctrl Pts',(-13.3882904778579,-10.4218393251423,-1.04083408558608E-16));
#9417=CARTESIAN_POINT('',(-15.675077185675,-11.5230977622533,0.));
#9418=CARTESIAN_POINT('Origin',(-15.,-10.,0.));
#9419=CARTESIAN_POINT('Ctrl Pts',(-15.6764092460936,-11.5258237909713,6.93889390390723E-17));
#9420=CARTESIAN_POINT('Ctrl Pts',(-15.1816817456953,-11.7444073771468,0.03632617514653));
#9421=CARTESIAN_POINT('Ctrl Pts',(-14.5700634637383,-11.7006543009145,0.0726523502930598));
#9422=CARTESIAN_POINT('Ctrl Pts',(-14.112175591995,-11.4128101852352,0.10897852543959));
#9423=CARTESIAN_POINT('Ctrl Pts',(-13.6452011738709,-11.119253952968,0.14602557461593));
#9424=CARTESIAN_POINT('Ctrl Pts',(-13.3381191053909,-10.5718228382361,0.183072623792269));
#9425=CARTESIAN_POINT('Ctrl Pts',(-13.3313947771057,-10.0204685483491,0.220119672968609));
#9426=CARTESIAN_POINT('Ctrl Pts',(-13.3246704488204,-9.46911425846216,0.257166722144949));
#9427=CARTESIAN_POINT('Ctrl Pts',(-13.6183038607298,-8.91383679342002,0.294213771321291));
#9428=CARTESIAN_POINT('Ctrl Pts',(-14.0779463710605,-8.6090816828823,0.331260820497631));
#9429=CARTESIAN_POINT('Ctrl Pts',(-14.5375888813912,-8.30432657234457,0.368307869673971));
#9430=CARTESIAN_POINT('Ctrl Pts',(-15.1632404901431,-8.25009381631124,0.405354918850311));
#9431=CARTESIAN_POINT('Ctrl Pts',(-15.6685313483052,-8.47104697428163,0.442401968026651));
#9432=CARTESIAN_POINT('Ctrl Pts',(-16.1738222064672,-8.69200013225201,0.47944901720299));
#9433=CARTESIAN_POINT('Ctrl Pts',(-16.5587523140395,-9.18813920422607,0.516496066379328));
#9434=CARTESIAN_POINT('Ctrl Pts',(-16.6471578533932,-9.73247249241234,0.553543115555668));
#9435=CARTESIAN_POINT('Ctrl Pts',(-16.6614257650046,-9.82032331374959,0.559522198167181));
#9436=CARTESIAN_POINT('Ctrl Pts',(-16.6679700273063,-9.90942946184446,0.565501280778695));
#9437=CARTESIAN_POINT('Ctrl Pts',(-16.6671910371619,-9.99865073764983,0.571480363390209));
#9438=CARTESIAN_POINT('Origin',(-15.,-10.,4.));
#9439=CARTESIAN_POINT('',(-16.6633491819668,-9.99963522328558,1.27148036339021));
#9440=CARTESIAN_POINT('',(-16.6649907850313,-10.0014379678122,1.07851963660979));
#9441=CARTESIAN_POINT('',(-16.666,-10.,4.));
#9442=CARTESIAN_POINT('Ctrl Pts',(-16.6649907850313,-10.0014379678122,1.07851963660979));
#9443=CARTESIAN_POINT('Ctrl Pts',(-16.6617723741096,-9.61090137508408,1.05243653366026));
#9444=CARTESIAN_POINT('Ctrl Pts',(-16.5246077727235,-9.21832985646356,1.02635343071072));
#9445=CARTESIAN_POINT('Ctrl Pts',(-16.2737775044129,-8.92195553365029,1.00027032776118));
#9446=CARTESIAN_POINT('Ctrl Pts',(-15.9175115607866,-8.50100124254812,0.96322327858484));
#9447=CARTESIAN_POINT('Ctrl Pts',(-15.3319382346072,-8.2741137068379,0.926176229408499));
#9448=CARTESIAN_POINT('Ctrl Pts',(-14.785052977246,-8.34515434993965,0.889129180232159));
#9449=CARTESIAN_POINT('Ctrl Pts',(-14.2381677198847,-8.4161949930414,0.852082131055818));
#9450=CARTESIAN_POINT('Ctrl Pts',(-13.7299705313417,-8.78516381495513,0.815035081879479));
#9451=CARTESIAN_POINT('Ctrl Pts',(-13.4930723773631,-9.28315331616688,0.777988032703139));
#9452=CARTESIAN_POINT('Ctrl Pts',(-13.2561742233845,-9.78114281737862,0.740940983526799));
#9453=CARTESIAN_POINT('Ctrl Pts',(-13.2905751039703,-10.4081529978884,0.703893934350459));
#9454=CARTESIAN_POINT('Ctrl Pts',(-13.5804932800309,-10.8772868894421,0.66684688517412));
#9455=CARTESIAN_POINT('Ctrl Pts',(-13.8704114560916,-11.3464207809959,0.629799835997779));
#9456=CARTESIAN_POINT('Ctrl Pts',(-14.4158469276272,-11.6576783835936,0.592752786821439));
#9457=CARTESIAN_POINT('Ctrl Pts',(-14.9672366648336,-11.6684613472114,0.555705737645099));
#9458=CARTESIAN_POINT('Ctrl Pts',(-15.51862640204,-11.6792443108291,0.518658688468759));
#9459=CARTESIAN_POINT('Ctrl Pts',(-16.0759704049172,-11.3895526354668,0.481611639292419));
#9460=CARTESIAN_POINT('Ctrl Pts',(-16.3840435298828,-10.9322477704337,0.444564590116079));
#9461=CARTESIAN_POINT('Ctrl Pts',(-16.5671141177547,-10.6604971252334,0.422549605613983));
#9462=CARTESIAN_POINT('Ctrl Pts',(-16.6621607121613,-10.3295579280615,0.400534621111888));
#9463=CARTESIAN_POINT('Ctrl Pts',(-16.6635932794994,-9.99933537909448,0.378519636609792));
#9464=CARTESIAN_POINT('Ctrl Pts',(-16.6671910371619,-9.99865073764983,0.571480363390209));
#9465=CARTESIAN_POINT('Ctrl Pts',(-16.6631433192538,-10.4622542356605,0.602548329955036));
#9466=CARTESIAN_POINT('Ctrl Pts',(-16.4613710696859,-10.9289661302211,0.633616296519864));
#9467=CARTESIAN_POINT('Ctrl Pts',(-16.118047013422,-11.2388249098967,0.664684263084691));
#9468=CARTESIAN_POINT('Ctrl Pts',(-15.7086496629616,-11.6083165347963,0.70173131226103));
#9469=CARTESIAN_POINT('Ctrl Pts',(-15.0979739909057,-11.7547722801968,0.738778361437369));
#9470=CARTESIAN_POINT('Ctrl Pts',(-14.5655171312584,-11.6111839010105,0.775825410613709));
#9471=CARTESIAN_POINT('Ctrl Pts',(-14.033060271611,-11.4675955218242,0.812872459790049));
#9472=CARTESIAN_POINT('Ctrl Pts',(-13.5788222243723,-11.033963018051,0.84991950896639));
#9473=CARTESIAN_POINT('Ctrl Pts',(-13.4106972420034,-10.5087402419385,0.886966558142731));
#9474=CARTESIAN_POINT('Ctrl Pts',(-13.2425722596345,-9.98351746582605,0.92401360731907));
#9475=CARTESIAN_POINT('Ctrl Pts',(-13.3605603421356,-9.36670441737438,0.961060656495409));
#9476=CARTESIAN_POINT('Ctrl Pts',(-13.7106614620273,-8.94061000038623,0.998107705671748));
#9477=CARTESIAN_POINT('Ctrl Pts',(-14.0607625819191,-8.51451558339806,1.03515475484809));
#9478=CARTESIAN_POINT('Ctrl Pts',(-14.6429767392015,-8.27913979787342,1.07220180402443));
#9479=CARTESIAN_POINT('Ctrl Pts',(-15.1908356179555,-8.34220651366761,1.10924885320077));
#9480=CARTESIAN_POINT('Ctrl Pts',(-15.7386944967096,-8.4052732294618,1.14629590237711));
#9481=CARTESIAN_POINT('Ctrl Pts',(-16.2521980969352,-8.76678244657481,1.18334295155345));
#9482=CARTESIAN_POINT('Ctrl Pts',(-16.4963261808093,-9.26128007721764,1.22039000072979));
#9483=CARTESIAN_POINT('Ctrl Pts',(-16.608549174885,-9.48859519718853,1.2374201216166));
#9484=CARTESIAN_POINT('Ctrl Pts',(-16.6638493580512,-9.74401262734354,1.2544502425034));
#9485=CARTESIAN_POINT('Ctrl Pts',(-16.6633491819668,-9.99963522328558,1.27148036339021));
#9486=CARTESIAN_POINT('Origin',(-15.,-10.,4.));
#9487=CARTESIAN_POINT('',(-16.6658558279687,-10.0015237952609,1.97148036339021));
#9488=CARTESIAN_POINT('',(-16.6687417861364,-9.99997573756952,1.7785196366098));
#9489=CARTESIAN_POINT('',(-16.666,-10.,4.));
#9490=CARTESIAN_POINT('Ctrl Pts',(-16.668741306591,-9.99997574181308,1.7785196366098));
#9491=CARTESIAN_POINT('Ctrl Pts',(-16.6688599435811,-9.44720213126613,1.74138549538496));
#9492=CARTESIAN_POINT('Ctrl Pts',(-16.3668274949188,-8.89454106233592,1.70425135416013));
#9493=CARTESIAN_POINT('Ctrl Pts',(-15.9017010646099,-8.59585115537534,1.6671172129353));
#9494=CARTESIAN_POINT('Ctrl Pts',(-15.4376655121909,-8.29786177668883,1.63007016375896));
#9495=CARTESIAN_POINT('Ctrl Pts',(-14.8113016140681,-8.2526536578585,1.59302311458262));
#9496=CARTESIAN_POINT('Ctrl Pts',(-14.3092835580737,-8.48091802869088,1.55597606540628));
#9497=CARTESIAN_POINT('Ctrl Pts',(-13.8072655020792,-8.70918239952326,1.51892901622994));
#9498=CARTESIAN_POINT('Ctrl Pts',(-13.4295932882132,-9.21091926001836,1.4818819670536));
#9499=CARTESIAN_POINT('Ctrl Pts',(-13.349120384328,-9.7564928551416,1.44483491787726));
#9500=CARTESIAN_POINT('Ctrl Pts',(-13.2686474804428,-10.3020664502648,1.40778786870092));
#9501=CARTESIAN_POINT('Ctrl Pts',(-13.4853738865385,-10.8914767800162,1.37074081952458));
#9502=CARTESIAN_POINT('Ctrl Pts',(-13.9001075103865,-11.2549637684195,1.33369377034824));
#9503=CARTESIAN_POINT('Ctrl Pts',(-14.3148411342344,-11.6184507568228,1.2966467211719));
#9504=CARTESIAN_POINT('Ctrl Pts',(-14.9275819758347,-11.7560144038781,1.25959967199556));
#9505=CARTESIAN_POINT('Ctrl Pts',(-15.4578920220932,-11.6046918718737,1.22255262281922));
#9506=CARTESIAN_POINT('Ctrl Pts',(-15.9882020683518,-11.4533693398692,1.18550557364288));
#9507=CARTESIAN_POINT('Ctrl Pts',(-16.4360813192687,-11.0131606288049,1.14845852446654));
#9508=CARTESIAN_POINT('Ctrl Pts',(-16.5965416641905,-10.4855457500257,1.1114114752902));
#9509=CARTESIAN_POINT('Ctrl Pts',(-16.6440293489689,-10.3293999492668,1.1004475290634));
#9510=CARTESIAN_POINT('Ctrl Pts',(-16.6663436334385,-10.1655987354384,1.08948358283659));
#9511=CARTESIAN_POINT('Ctrl Pts',(-16.6649907850313,-10.0014379678122,1.07851963660979));
#9512=CARTESIAN_POINT('Ctrl Pts',(-16.6633491819668,-9.99963522328558,1.27148036339021));
#9513=CARTESIAN_POINT('Ctrl Pts',(-16.6627612830976,-10.3000898827778,1.29149729167974));
#9514=CARTESIAN_POINT('Ctrl Pts',(-16.5850836763294,-10.6008279843625,1.31151421996927));
#9515=CARTESIAN_POINT('Ctrl Pts',(-16.4321390262416,-10.8565494596152,1.33153114825881));
#9516=CARTESIAN_POINT('Ctrl Pts',(-16.1490712202775,-11.3298351671973,1.36857819743515));
#9517=CARTESIAN_POINT('Ctrl Pts',(-15.6081830408266,-11.6489205381888,1.40562524661149));
#9518=CARTESIAN_POINT('Ctrl Pts',(-15.0570283710643,-11.6677669144638,1.44267229578783));
#9519=CARTESIAN_POINT('Ctrl Pts',(-14.505873701302,-11.6866132907387,1.47971934496417));
#9520=CARTESIAN_POINT('Ctrl Pts',(-13.9444525412283,-11.4052206722971,1.51676639414051));
#9521=CARTESIAN_POINT('Ctrl Pts',(-13.6297162289666,-10.9523766872749,1.55381344331685));
#9522=CARTESIAN_POINT('Ctrl Pts',(-13.3149799167049,-10.4995327022527,1.59086049249319));
#9523=CARTESIAN_POINT('Ctrl Pts',(-13.2469284522552,-9.87523735064986,1.62790754166953));
#9524=CARTESIAN_POINT('Ctrl Pts',(-13.4567076604804,-9.36521838263765,1.66495459084587));
#9525=CARTESIAN_POINT('Ctrl Pts',(-13.6664868687056,-8.85519941462545,1.70200164002221));
#9526=CARTESIAN_POINT('Ctrl Pts',(-14.1540967496057,-8.45945683020384,1.73904868919855));
#9527=CARTESIAN_POINT('Ctrl Pts',(-14.6963678920727,-8.35911413114816,1.77609573837489));
#9528=CARTESIAN_POINT('Ctrl Pts',(-15.2386390345398,-8.25877143209247,1.81314278755123));
#9529=CARTESIAN_POINT('Ctrl Pts',(-15.8355714385739,-8.45382861840273,1.85018983672757));
#9530=CARTESIAN_POINT('Ctrl Pts',(-16.213960946897,-8.85501190072828,1.88723688590391));
#9531=CARTESIAN_POINT('Ctrl Pts',(-16.5007750453132,-9.15910336967454,1.91531804506601));
#9532=CARTESIAN_POINT('Ctrl Pts',(-16.6620267716353,-9.58162322075589,1.94339920422811));
#9533=CARTESIAN_POINT('Ctrl Pts',(-16.6658558279687,-10.0015237952609,1.97148036339021));
#9534=CARTESIAN_POINT('Origin',(-15.,-10.,4.));
#9535=CARTESIAN_POINT('',(-16.6685090241476,-9.99943625435561,2.67148036339021));
#9536=CARTESIAN_POINT('',(-16.66492032495,-9.99857774531074,2.47851963660979));
#9537=CARTESIAN_POINT('',(-16.666,-10.,4.));
#9538=CARTESIAN_POINT('Ctrl Pts',(-16.66492032495,-9.99857774531074,2.47851963660979));
#9539=CARTESIAN_POINT('Ctrl Pts',(-16.6662755099423,-9.83179018295812,2.46738150628601));
#9540=CARTESIAN_POINT('Ctrl Pts',(-16.6432317570283,-9.66536855851988,2.45624337596222));
#9541=CARTESIAN_POINT('Ctrl Pts',(-16.594245932966,-9.50696967861907,2.44510524563844));
#9542=CARTESIAN_POINT('Ctrl Pts',(-16.4313119233769,-8.98011185575535,2.4080581964621));
#9543=CARTESIAN_POINT('Ctrl Pts',(-15.9813743433956,-8.54201164647713,2.37101114728576));
#9544=CARTESIAN_POINT('Ctrl Pts',(-15.4503607308701,-8.39317885267126,2.33396409810942));
#9545=CARTESIAN_POINT('Ctrl Pts',(-14.9193471183446,-8.24434605886539,2.29691704893308));
#9546=CARTESIAN_POINT('Ctrl Pts',(-14.307257473275,-8.38478068053188,2.25986999975674));
#9547=CARTESIAN_POINT('Ctrl Pts',(-13.8942331229627,-8.75020857436374,2.2228229505804));
#9548=CARTESIAN_POINT('Ctrl Pts',(-13.4812087726504,-9.1156364681956,2.18577590140406));
#9549=CARTESIAN_POINT('Ctrl Pts',(-13.2672497170955,-9.70605763419282,2.14872885222772));
#9550=CARTESIAN_POINT('Ctrl Pts',(-13.3502807933188,-10.2512479626338,2.11168180305138));
#9551=CARTESIAN_POINT('Ctrl Pts',(-13.433311869542,-10.7964382910748,2.07463475387504));
#9552=CARTESIAN_POINT('Ctrl Pts',(-13.8133330775434,-11.2963977819595,2.0375877046987));
#9553=CARTESIAN_POINT('Ctrl Pts',(-14.3164162094338,-11.5223048855013,2.00054065552236));
#9554=CARTESIAN_POINT('Ctrl Pts',(-14.8194993413241,-11.7482119890431,1.96349360634602));
#9555=CARTESIAN_POINT('Ctrl Pts',(-15.4456443971033,-11.700066705242,1.92644655716968));
#9556=CARTESIAN_POINT('Ctrl Pts',(-15.9082771879223,-11.3999041282926,1.88939950799334));
#9557=CARTESIAN_POINT('Ctrl Pts',(-16.3698223985333,-11.1004471884798,1.85243955086549));
#9558=CARTESIAN_POINT('Ctrl Pts',(-16.6686232260882,-10.5501564723576,1.81547959373764));
#9559=CARTESIAN_POINT('Ctrl Pts',(-16.668741306591,-9.99997574181308,1.7785196366098));
#9560=CARTESIAN_POINT('Ctrl Pts',(-16.6658558279687,-10.0015237952609,1.97148036339021));
#9561=CARTESIAN_POINT('Ctrl Pts',(-16.6670783878262,-10.1355917069947,1.98044625340445));
#9562=CARTESIAN_POINT('Ctrl Pts',(-16.6522528327537,-10.2693926022211,1.98941214341869));
#9563=CARTESIAN_POINT('Ctrl Pts',(-16.6203421479384,-10.3989865235809,1.99837803343293));
#9564=CARTESIAN_POINT('Ctrl Pts',(-16.4884872280444,-10.9344684857673,2.03542508260927));
#9565=CARTESIAN_POINT('Ctrl Pts',(-16.0649307756441,-11.3981230317991,2.07247213178561));
#9566=CARTESIAN_POINT('Ctrl Pts',(-15.5435262072274,-11.5777446491442,2.10951918096195));
#9567=CARTESIAN_POINT('Ctrl Pts',(-15.0221216388108,-11.7573662664892,2.14656623013829));
#9568=CARTESIAN_POINT('Ctrl Pts',(-14.4028689543777,-11.6529549551475,2.18361327931463));
#9569=CARTESIAN_POINT('Ctrl Pts',(-13.9691878657227,-11.3122977043507,2.22066032849097));
#9570=CARTESIAN_POINT('Ctrl Pts',(-13.5355067770677,-10.9716404535538,2.25770737766731));
#9571=CARTESIAN_POINT('Ctrl Pts',(-13.2873972841907,-10.3947372633017,2.29475442684365));
#9572=CARTESIAN_POINT('Ctrl Pts',(-13.3384141976562,-9.84562532165677,2.33180147601999));
#9573=CARTESIAN_POINT('Ctrl Pts',(-13.3894311111217,-9.29651338001179,2.36884852519633));
#9574=CARTESIAN_POINT('Ctrl Pts',(-13.7395744309295,-8.77519268697389,2.40589557437267));
#9575=CARTESIAN_POINT('Ctrl Pts',(-14.2285904810596,-8.52026141726962,2.44294262354901));
#9576=CARTESIAN_POINT('Ctrl Pts',(-14.7176065311896,-8.26533014756536,2.47998967272535));
#9577=CARTESIAN_POINT('Ctrl Pts',(-15.3454953116418,-8.27678830119472,2.51703672190169));
#9578=CARTESIAN_POINT('Ctrl Pts',(-15.8248845397239,-8.54939170829145,2.55408377107803));
#9579=CARTESIAN_POINT('Ctrl Pts',(-16.3042737678059,-8.82199511538819,2.59113082025437));
#9580=CARTESIAN_POINT('Ctrl Pts',(-16.6351634435178,-9.3557437759523,2.62817786943071));
#9581=CARTESIAN_POINT('Ctrl Pts',(-16.6661119032437,-9.90635147885495,2.66522491860705));
#9582=CARTESIAN_POINT('Ctrl Pts',(-16.6678537997891,-9.93734176606421,2.6673100668681));
#9583=CARTESIAN_POINT('Ctrl Pts',(-16.6686455231177,-9.96838546044008,2.66939521512916));
#9584=CARTESIAN_POINT('Ctrl Pts',(-16.6685090241476,-9.99943625435561,2.67148036339021));
#9585=CARTESIAN_POINT('Origin',(-15.,-10.,4.));
#9586=CARTESIAN_POINT('',(-16.6641896916198,-9.99883056905918,3.37148036339021));
#9587=CARTESIAN_POINT('',(-16.6637100014683,-10.0008527826236,3.17851963660979));
#9588=CARTESIAN_POINT('',(-16.666,-10.,4.));
#9589=CARTESIAN_POINT('Ctrl Pts',(-16.6637100014683,-10.0008527826236,3.17851963660979));
#9590=CARTESIAN_POINT('Ctrl Pts',(-16.6621664007059,-9.66797331594755,3.15633046801071));
#9591=CARTESIAN_POINT('Ctrl Pts',(-16.56543951406,-9.33426787425992,3.13414129941163));
#9592=CARTESIAN_POINT('Ctrl Pts',(-16.379615276458,-9.06119188318812,3.11195213081255));
#9593=CARTESIAN_POINT('Ctrl Pts',(-16.0693630181159,-8.60526404502054,3.07490508163621));
#9594=CARTESIAN_POINT('Ctrl Pts',(-15.5107459993938,-8.31834481162707,3.03785803245988));
#9595=CARTESIAN_POINT('Ctrl Pts',(-14.9594321871066,-8.3317514442721,3.00081098328354));
#9596=CARTESIAN_POINT('Ctrl Pts',(-14.4081183748194,-8.34515807691714,2.9637639341072));
#9597=CARTESIAN_POINT('Ctrl Pts',(-13.864107768967,-8.65889057560069,2.92671688493085));
#9598=CARTESIAN_POINT('Ctrl Pts',(-13.5763832698313,-9.12935977764045,2.88966983575451));
#9599=CARTESIAN_POINT('Ctrl Pts',(-13.2886587706957,-9.59982897968023,2.85262278657817));
#9600=CARTESIAN_POINT('Ctrl Pts',(-13.2572203782769,-10.2270348850762,2.81557573740184));
#9601=CARTESIAN_POINT('Ctrl Pts',(-13.4964568234424,-10.7239177492225,2.7785286882255));
#9602=CARTESIAN_POINT('Ctrl Pts',(-13.7356932686079,-11.2208006133687,2.74148163904916));
#9603=CARTESIAN_POINT('Ctrl Pts',(-14.2456045513576,-11.5873604362652,2.70443458987282));
#9604=CARTESIAN_POINT('Ctrl Pts',(-14.792814357206,-11.6558300335834,2.66738754069648));
#9605=CARTESIAN_POINT('Ctrl Pts',(-15.3400241630545,-11.7242996309016,2.63034049152013));
#9606=CARTESIAN_POINT('Ctrl Pts',(-15.9245324920015,-11.4946790026414,2.5932934423438));
#9607=CARTESIAN_POINT('Ctrl Pts',(-16.2788214368767,-11.0720609702867,2.55624639316746));
#9608=CARTESIAN_POINT('Ctrl Pts',(-16.5265940321902,-10.7765023077388,2.5303374743149));
#9609=CARTESIAN_POINT('Ctrl Pts',(-16.6617679666121,-10.3865499895734,2.50442855546235));
#9610=CARTESIAN_POINT('Ctrl Pts',(-16.66492032495,-9.99857774531074,2.47851963660979));
#9611=CARTESIAN_POINT('Ctrl Pts',(-16.6685090241476,-9.99943625435561,2.67148036339021));
#9612=CARTESIAN_POINT('Ctrl Pts',(-16.6662203315139,-10.5200681923775,2.7064422643055));
#9613=CARTESIAN_POINT('Ctrl Pts',(-16.4029750948965,-11.0426960653573,2.74140416522078));
#9614=CARTESIAN_POINT('Ctrl Pts',(-15.9822463015998,-11.3490334030561,2.77636606613607));
#9615=CARTESIAN_POINT('Ctrl Pts',(-15.5364249964903,-11.6736408791134,2.81341311531241));
#9616=CARTESIAN_POINT('Ctrl Pts',(-14.9137751425314,-11.7553890859868,2.85046016448875));
#9617=CARTESIAN_POINT('Ctrl Pts',(-14.3992712693864,-11.5568634853063,2.88750721366509));
#9618=CARTESIAN_POINT('Ctrl Pts',(-13.8847673962414,-11.3583378846257,2.92455426284143));
#9619=CARTESIAN_POINT('Ctrl Pts',(-13.4784095039101,-10.8795384763911,2.96160131201777));
#9620=CARTESIAN_POINT('Ctrl Pts',(-13.3661795668735,-10.3396022849287,2.99864836119411));
#9621=CARTESIAN_POINT('Ctrl Pts',(-13.2539496298369,-9.7996660934662,3.03569541037045));
#9622=CARTESIAN_POINT('Ctrl Pts',(-13.4358476480949,-9.19859311877586,3.07274245954679));
#9623=CARTESIAN_POINT('Ctrl Pts',(-13.828622494431,-8.81148257939958,3.10978950872313));
#9624=CARTESIAN_POINT('Ctrl Pts',(-14.2213973407671,-8.42437204002329,3.14683655789947));
#9625=CARTESIAN_POINT('Ctrl Pts',(-14.8250490151812,-8.25122393596108,3.18388360707581));
#9626=CARTESIAN_POINT('Ctrl Pts',(-15.3632980792249,-8.37128473167712,3.22093065625215));
#9627=CARTESIAN_POINT('Ctrl Pts',(-15.9015471432685,-8.49134552739316,3.25797770542849));
#9628=CARTESIAN_POINT('Ctrl Pts',(-16.3743935969416,-8.90461522288745,3.29502475460483));
#9629=CARTESIAN_POINT('Ctrl Pts',(-16.5654249655814,-9.4219484480033,3.33207180378117));
#9630=CARTESIAN_POINT('Ctrl Pts',(-16.6331610943294,-9.60538507514802,3.34520799031751));
#9631=CARTESIAN_POINT('Ctrl Pts',(-16.6654652280384,-9.80190538255376,3.35834417685386));
#9632=CARTESIAN_POINT('Ctrl Pts',(-16.6641896916198,-9.99883056905918,3.37148036339021));
#9633=CARTESIAN_POINT('Origin',(-15.,-10.,4.));
#9634=CARTESIAN_POINT('',(-16.6642806992699,-10.0012124486558,4.07148036339022));
#9635=CARTESIAN_POINT('',(-16.6680323256648,-10.0009660456509,3.8785196366098));
#9636=CARTESIAN_POINT('',(-16.666,-10.,4.));
#9637=CARTESIAN_POINT('Ctrl Pts',(-16.6680323256648,-10.0009660456509,3.8785196366098));
#9638=CARTESIAN_POINT('Ctrl Pts',(-16.6646132194972,-9.50559820416748,3.84527942973542));
#9639=CARTESIAN_POINT('Ctrl Pts',(-16.4297940876874,-9.00741573513633,3.81203922286105));
#9640=CARTESIAN_POINT('Ctrl Pts',(-16.0437119187986,-8.6979383955612,3.77879901598668));
#9641=CARTESIAN_POINT('Ctrl Pts',(-15.613413601132,-8.35301809282261,3.74175196681034));
#9642=CARTESIAN_POINT('Ctrl Pts',(-14.995221408247,-8.24250097761573,3.704704917634));
#9643=CARTESIAN_POINT('Ctrl Pts',(-14.4720696864628,-8.41696854887757,3.66765786845765));
#9644=CARTESIAN_POINT('Ctrl Pts',(-13.9489179646786,-8.59143612013942,3.63061081928131));
#9645=CARTESIAN_POINT('Ctrl Pts',(-13.5208067139953,-9.05088837786998,3.59356377010497));
#9646=CARTESIAN_POINT('Ctrl Pts',(-13.3836739909864,-9.58504310611734,3.55651672092863));
#9647=CARTESIAN_POINT('Ctrl Pts',(-13.2465412679775,-10.1191978343647,3.51946967175229));
#9648=CARTESIAN_POINT('Ctrl Pts',(-13.4003870726431,-10.7280550331288,3.48242262257595));
#9649=CARTESIAN_POINT('Ctrl Pts',(-13.7747992213996,-11.1329527983623,3.44537557339961));
#9650=CARTESIAN_POINT('Ctrl Pts',(-14.1492113701561,-11.5378505635958,3.40832852422327));
#9651=CARTESIAN_POINT('Ctrl Pts',(-14.7441898630034,-11.7387888952986,3.37128147504694));
#9652=CARTESIAN_POINT('Ctrl Pts',(-15.2874248052393,-11.6438022911897,3.3342344258706));
#9653=CARTESIAN_POINT('Ctrl Pts',(-15.8306597474752,-11.5488156870807,3.29718737669426));
#9654=CARTESIAN_POINT('Ctrl Pts',(-16.3221511390998,-11.1579041471599,3.26014032751792));
#9655=CARTESIAN_POINT('Ctrl Pts',(-16.536953085931,-10.6499801557287,3.22309327834158));
#9656=CARTESIAN_POINT('Ctrl Pts',(-16.6231003431279,-10.4462750246914,3.20823539776432));
#9657=CARTESIAN_POINT('Ctrl Pts',(-16.6647435974628,-10.2237490727847,3.19337751718705));
#9658=CARTESIAN_POINT('Ctrl Pts',(-16.6637100014683,-10.0008527826236,3.17851963660979));
#9659=CARTESIAN_POINT('Ctrl Pts',(-16.6641896916198,-9.99883056905918,3.37148036339021));
#9660=CARTESIAN_POINT('Ctrl Pts',(-16.6618679237299,-10.3572794287687,3.3953912260302));
#9661=CARTESIAN_POINT('Ctrl Pts',(-16.548288911008,-10.7170697469545,3.4193020886702));
#9662=CARTESIAN_POINT('Ctrl Pts',(-16.3346237287904,-11.0017377012874,3.44321295131019));
#9663=CARTESIAN_POINT('Ctrl Pts',(-16.0035748397532,-11.4427969747182,3.48026000048653));
#9664=CARTESIAN_POINT('Ctrl Pts',(-15.4322607780725,-11.7035187668424,3.51730704966287));
#9665=CARTESIAN_POINT('Ctrl Pts',(-14.8821606960968,-11.6645758673272,3.55435409883921));
#9666=CARTESIAN_POINT('Ctrl Pts',(-14.3320606141211,-11.6256329678119,3.59140114801554));
#9667=CARTESIAN_POINT('Ctrl Pts',(-13.8031745118505,-11.2870253766572,3.62844819719188));
#9668=CARTESIAN_POINT('Ctrl Pts',(-13.5375631033236,-10.8037270947724,3.66549524636822));
#9669=CARTESIAN_POINT('Ctrl Pts',(-13.2719516947968,-10.3204288128875,3.70254229554456));
#9670=CARTESIAN_POINT('Ctrl Pts',(-13.2696149800139,-9.69243984027253,3.73958934472091));
#9671=CARTESIAN_POINT('Ctrl Pts',(-13.5316224271389,-9.2071783156661,3.77663639389725));
#9672=CARTESIAN_POINT('Ctrl Pts',(-13.7936298742639,-8.72191679105968,3.81368344307359));
#9673=CARTESIAN_POINT('Ctrl Pts',(-14.3199814832969,-8.37938271446182,3.85073049224993));
#9674=CARTESIAN_POINT('Ctrl Pts',(-14.8697765276525,-8.33634716155033,3.88777754142627));
#9675=CARTESIAN_POINT('Ctrl Pts',(-15.419571572008,-8.29331160863883,3.92482459060261));
#9676=CARTESIAN_POINT('Ctrl Pts',(-15.9928100516862,-8.54977457941371,3.96187163977894));
#9677=CARTESIAN_POINT('Ctrl Pts',(-16.3271320462624,-8.98835804188682,3.99891868895528));
#9678=CARTESIAN_POINT('Ctrl Pts',(-16.5454037149127,-9.27469978951192,4.02310591376693));
#9679=CARTESIAN_POINT('Ctrl Pts',(-16.6618371270144,-9.63867047659017,4.04729313857857));
#9680=CARTESIAN_POINT('Ctrl Pts',(-16.6642806992699,-10.0012124486558,4.07148036339022));
#9681=CARTESIAN_POINT('Origin',(-15.,-10.,4.));
#9682=CARTESIAN_POINT('',(-16.6685641984665,-10.0004924312751,4.77148036339021));
#9683=CARTESIAN_POINT('',(-16.6666360603741,-9.99853839705222,4.5785196366098));
#9684=CARTESIAN_POINT('',(-16.666,-10.,4.));
#9685=CARTESIAN_POINT('Ctrl Pts',(-16.6666360603741,-9.99853839705222,4.5785196366098));
#9686=CARTESIAN_POINT('Ctrl Pts',(-16.6676284318155,-9.89034513840702,4.57127544063647));
#9687=CARTESIAN_POINT('Ctrl Pts',(-16.6579946985884,-9.78232782481888,4.56403124466314));
#9688=CARTESIAN_POINT('Ctrl Pts',(-16.6370921504892,-9.67653704694216,4.55678704868981));
#9689=CARTESIAN_POINT('Ctrl Pts',(-16.5301958530681,-9.13551963592343,4.51973999951347));
#9690=CARTESIAN_POINT('Ctrl Pts',(-16.1285826105747,-8.65273353053979,4.48269295033713));
#9691=CARTESIAN_POINT('Ctrl Pts',(-15.6160628650447,-8.44914038755636,4.44564590116079));
#9692=CARTESIAN_POINT('Ctrl Pts',(-15.1035431195147,-8.24554724457292,4.40859885198445));
#9693=CARTESIAN_POINT('Ctrl Pts',(-14.4801168709481,-8.32114706398968,4.37155180280812));
#9694=CARTESIAN_POINT('Ctrl Pts',(-14.031113989483,-8.64133930290906,4.33450475363177));
#9695=CARTESIAN_POINT('Ctrl Pts',(-13.582111108018,-8.96153154182844,4.29745770445543));
#9696=CARTESIAN_POINT('Ctrl Pts',(-13.3075315936544,-9.52631620025045,4.26041065527909));
#9697=CARTESIAN_POINT('Ctrl Pts',(-13.3330450622543,-10.0772025046255,4.22336360610275));
#9698=CARTESIAN_POINT('Ctrl Pts',(-13.3585585308543,-10.6280888090006,4.18631655692641));
#9699=CARTESIAN_POINT('Ctrl Pts',(-13.6841649824178,-11.1650767593287,4.14926950775007));
#9700=CARTESIAN_POINT('Ctrl Pts',(-14.160840780622,-11.4423975858716,4.11222245857374));
#9701=CARTESIAN_POINT('Ctrl Pts',(-14.6375165788261,-11.7197184124145,4.0751754093974));
#9702=CARTESIAN_POINT('Ctrl Pts',(-15.265261723671,-11.7373721151722,4.03812836022106));
#9703=CARTESIAN_POINT('Ctrl Pts',(-15.7567696715678,-11.4872789433695,4.00108131104471));
#9704=CARTESIAN_POINT('Ctrl Pts',(-16.2482776194645,-11.2371857715668,3.96403426186837));
#9705=CARTESIAN_POINT('Ctrl Pts',(-16.6035483704131,-10.7193457252036,3.92698721269203));
#9706=CARTESIAN_POINT('Ctrl Pts',(-16.6599815246633,-10.1707639568869,3.88994016351569));
#9707=CARTESIAN_POINT('Ctrl Pts',(-16.6657804242682,-10.1143933598178,3.88613332121373));
#9708=CARTESIAN_POINT('Ctrl Pts',(-16.6684238995814,-10.0576981611013,3.88232647891176));
#9709=CARTESIAN_POINT('Ctrl Pts',(-16.6680323256648,-10.0009660456509,3.8785196366098));
#9710=CARTESIAN_POINT('Ctrl Pts',(-16.6642806992699,-10.0012124486558,4.07148036339022));
#9711=CARTESIAN_POINT('Ctrl Pts',(-16.665579893794,-10.1939681749494,4.08434018775491));
#9712=CARTESIAN_POINT('Ctrl Pts',(-16.6346562245379,-10.3863200293777,4.09720001211961));
#9713=CARTESIAN_POINT('Ctrl Pts',(-16.5696833589659,-10.5663859745943,4.11005983648431));
#9714=CARTESIAN_POINT('Ctrl Pts',(-16.382507167619,-11.0851264906573,4.14710688566065));
#9715=CARTESIAN_POINT('Ctrl Pts',(-15.9127492754508,-11.5019035686119,4.18415393483698));
#9716=CARTESIAN_POINT('Ctrl Pts',(-15.3754085835772,-11.6259665786876,4.22120098401332));
#9717=CARTESIAN_POINT('Ctrl Pts',(-14.8380678917035,-11.7500295887632,4.25824803318966));
#9718=CARTESIAN_POINT('Ctrl Pts',(-14.2331444001243,-11.5813785309599,4.29529508236601));
#9719=CARTESIAN_POINT('Ctrl Pts',(-13.8374996328648,-11.1972016605574,4.33234213154235));
#9720=CARTESIAN_POINT('Ctrl Pts',(-13.4418548656054,-10.8130247901549,4.36938918071869));
#9721=CARTESIAN_POINT('Ctrl Pts',(-13.2554888226657,-10.2133221071532,4.40643622989502));
#9722=CARTESIAN_POINT('Ctrl Pts',(-13.3636975578329,-9.67256567469336,4.44348327907136));
#9723=CARTESIAN_POINT('Ctrl Pts',(-13.471906293,-9.13180924223355,4.4805303282477));
#9724=CARTESIAN_POINT('Ctrl Pts',(-13.8746898062741,-8.64999906031561,4.51757737742405));
#9725=CARTESIAN_POINT('Ctrl Pts',(-14.387702045816,-8.44765012483052,4.55462442660039));
#9726=CARTESIAN_POINT('Ctrl Pts',(-14.900714285358,-8.24530118934543,4.59167147577673));
#9727=CARTESIAN_POINT('Ctrl Pts',(-15.5239552511679,-8.3224135002932,4.62871852495307));
#9728=CARTESIAN_POINT('Ctrl Pts',(-15.9721798733629,-8.64369427729152,4.6657655741294));
#9729=CARTESIAN_POINT('Ctrl Pts',(-16.398520364984,-8.94928883330469,4.70100383721634));
#9730=CARTESIAN_POINT('Ctrl Pts',(-16.6665173165624,-9.47579132558647,4.73624210030327));
#9731=CARTESIAN_POINT('Ctrl Pts',(-16.6685641984665,-10.0004924312751,4.77148036339021));
#9732=CARTESIAN_POINT('Origin',(-15.,-10.,4.));
#9733=CARTESIAN_POINT('',(-16.6657318647841,-9.99847819321684,5.47148036339021));
#9734=CARTESIAN_POINT('',(-16.6632775623115,-9.9999437523457,5.2785196366098));
#9735=CARTESIAN_POINT('',(-16.666,-10.,4.));
#9736=CARTESIAN_POINT('Ctrl Pts',(-16.6632775623115,-9.9999437523457,5.2785196366098));
#9737=CARTESIAN_POINT('Ctrl Pts',(-16.6633602649375,-9.72530233420805,5.26022440236118));
#9738=CARTESIAN_POINT('Ctrl Pts',(-16.5991043467443,-9.45069734119511,5.24192916811256));
#9739=CARTESIAN_POINT('Ctrl Pts',(-16.4702970143586,-9.210743590017,5.22363393386394));
#9740=CARTESIAN_POINT('Ctrl Pts',(-16.2094677999131,-8.72484773871831,5.1865868846876));
#9741=CARTESIAN_POINT('Ctrl Pts',(-15.6839488768039,-8.3810374981041,5.14953983551125));
#9742=CARTESIAN_POINT('Ctrl Pts',(-15.134259867688,-8.33666801895819,5.11249278633491));
#9743=CARTESIAN_POINT('Ctrl Pts',(-14.584570858572,-8.29229853981227,5.07544573715857));
#9744=CARTESIAN_POINT('Ctrl Pts',(-14.0107117634493,-8.54736982213464,5.03839868798223));
#9745=CARTESIAN_POINT('Ctrl Pts',(-13.6753265461866,-8.98514078219886,5.00135163880589));
#9746=CARTESIAN_POINT('Ctrl Pts',(-13.3399413289238,-9.42291174226308,4.96430458962955));
#9747=CARTESIAN_POINT('Ctrl Pts',(-13.2430299895211,-10.0433823800691,4.92725754045321));
#9748=CARTESIAN_POINT('Ctrl Pts',(-13.4289469322776,-10.562575550115,4.89021049127687));
#9749=CARTESIAN_POINT('Ctrl Pts',(-13.6148638750341,-11.0817687201609,4.85316344210053));
#9750=CARTESIAN_POINT('Ctrl Pts',(-14.0836090999499,-11.4996844224466,4.81611639292419));
#9751=CARTESIAN_POINT('Ctrl Pts',(-14.6206471836982,-11.6250509013455,4.77906934374785));
#9752=CARTESIAN_POINT('Ctrl Pts',(-15.1576852674464,-11.7504173802444,4.74202229457151));
#9753=CARTESIAN_POINT('Ctrl Pts',(-15.7630162100271,-11.5832346357565,4.70497524539517));
#9754=CARTESIAN_POINT('Ctrl Pts',(-16.1595920051431,-11.2000189051856,4.66792819621883));
#9755=CARTESIAN_POINT('Ctrl Pts',(-16.4786211982497,-10.8917373438411,4.63812534301582));
#9756=CARTESIAN_POINT('Ctrl Pts',(-16.6625534126244,-10.4436489126747,4.60832248981281));
#9757=CARTESIAN_POINT('Ctrl Pts',(-16.6666360603741,-9.99853839705222,4.5785196366098));
#9758=CARTESIAN_POINT('Ctrl Pts',(-16.6685641984665,-10.0004924312751,4.77148036339021));
#9759=CARTESIAN_POINT('Ctrl Pts',(-16.6686692652657,-10.027425429043,4.77328914947961));
#9760=CARTESIAN_POINT('Ctrl Pts',(-16.6680736104087,-10.0543536805418,4.77509793556902));
#9761=CARTESIAN_POINT('Ctrl Pts',(-16.6667626807532,-10.0812470656621,4.77690672165842));
#9762=CARTESIAN_POINT('Ctrl Pts',(-16.6399125873683,-10.6320698339855,4.81395377083476));
#9763=CARTESIAN_POINT('Ctrl Pts',(-16.3130041220183,-11.1682661275834,4.85100082001111));
#9764=CARTESIAN_POINT('Ctrl Pts',(-15.8356568269973,-11.4444295023148,4.88804786918745));
#9765=CARTESIAN_POINT('Ctrl Pts',(-15.3583095319764,-11.7205928770462,4.92509491836379));
#9766=CARTESIAN_POINT('Ctrl Pts',(-14.7305234072845,-11.736723332911,4.96214196754013));
#9767=CARTESIAN_POINT('Ctrl Pts',(-14.2396237521779,-11.485438279201,4.99918901671646));
#9768=CARTESIAN_POINT('Ctrl Pts',(-13.7487240970713,-11.234153225491,5.0362360658928));
#9769=CARTESIAN_POINT('Ctrl Pts',(-13.3947109115499,-10.7154526622061,5.07328311506915));
#9770=CARTESIAN_POINT('Ctrl Pts',(-13.3396090325246,-10.1667355833913,5.11033016424549));
#9771=CARTESIAN_POINT('Ctrl Pts',(-13.2845071534992,-9.61801850457656,5.14737721342183));
#9772=CARTESIAN_POINT('Ctrl Pts',(-13.52831658097,-9.03928491023192,5.18442426259817));
#9773=CARTESIAN_POINT('Ctrl Pts',(-13.9594505595911,-8.6954097264222,5.22147131177451));
#9774=CARTESIAN_POINT('Ctrl Pts',(-14.3905845382122,-8.35153454261247,5.25851836095085));
#9775=CARTESIAN_POINT('Ctrl Pts',(-15.0090430679838,-8.24251776933766,5.29556541012719));
#9776=CARTESIAN_POINT('Ctrl Pts',(-15.5317699054477,-8.41825422814124,5.33261245930353));
#9777=CARTESIAN_POINT('Ctrl Pts',(-16.0544967429115,-8.59399068694482,5.36965950847986));
#9778=CARTESIAN_POINT('Ctrl Pts',(-16.4814918880678,-9.0544803778268,5.4067065576562));
#9779=CARTESIAN_POINT('Ctrl Pts',(-16.6173281038004,-9.5889662732554,5.44375360683254));
#9780=CARTESIAN_POINT('Ctrl Pts',(-16.6512156222314,-9.72230627050696,5.45299585901843));
#9781=CARTESIAN_POINT('Ctrl Pts',(-16.6669822934182,-9.86025156673352,5.46223811120432));
#9782=CARTESIAN_POINT('Ctrl Pts',(-16.6657318647841,-9.99847819321684,5.47148036339021));
#9783=CARTESIAN_POINT('Origin',(-15.,-10.,4.));
#9784=CARTESIAN_POINT('',(-16.6633787344493,-10.0004304228837,6.17148036339021));
#9785=CARTESIAN_POINT('',(-16.6664295714326,-10.0014906689886,5.9785196366098));
#9786=CARTESIAN_POINT('',(-16.666,-10.,4.));
#9787=CARTESIAN_POINT('Ctrl Pts',(-16.6664295714326,-10.0014906689886,5.9785196366098));
#9788=CARTESIAN_POINT('Ctrl Pts',(-16.6623836036609,-9.56305953449899,5.94917336408588));
#9789=CARTESIAN_POINT('Ctrl Pts',(-16.4846437757866,-9.1217262956008,5.91982709156197));
#9790=CARTESIAN_POINT('Ctrl Pts',(-16.1742579544333,-8.81432835748561,5.89048081903805));
#9791=CARTESIAN_POINT('Ctrl Pts',(-15.7824235646333,-8.42626590353074,5.85343376986171));
#9792=CARTESIAN_POINT('Ctrl Pts',(-15.179193796671,-8.2516535720841,5.81638672068537));
#9793=CARTESIAN_POINT('Ctrl Pts',(-14.6406549885415,-8.37040797887343,5.77933967150903));
#9794=CARTESIAN_POINT('Ctrl Pts',(-14.1021161804119,-8.48916238566276,5.74229262233269));
#9795=CARTESIAN_POINT('Ctrl Pts',(-13.6282683321152,-8.90128353068805,5.70524557315636));
#9796=CARTESIAN_POINT('Ctrl Pts',(-13.4359822379784,-9.4181517109175,5.66819852398001));
#9797=CARTESIAN_POINT('Ctrl Pts',(-13.2436961438415,-9.93501989114696,5.63115147480367));
#9798=CARTESIAN_POINT('Ctrl Pts',(-13.3329718038647,-10.5566351065806,5.59410442562733));
#9799=CARTESIAN_POINT('Ctrl Pts',(-13.6629495126592,-10.9984963620356,5.55705737645099));
#9800=CARTESIAN_POINT('Ctrl Pts',(-13.9929272214536,-11.4403576174907,5.52001032727465));
#9801=CARTESIAN_POINT('Ctrl Pts',(-14.5636069790195,-11.7024649129672,5.48296327809831));
#9802=CARTESIAN_POINT('Ctrl Pts',(-15.1137999417662,-11.6648569201785,5.44591622892197));
#9803=CARTESIAN_POINT('Ctrl Pts',(-15.6639929045129,-11.6272489273898,5.40886917974563));
#9804=CARTESIAN_POINT('Ctrl Pts',(-16.1936990724405,-11.2899256463359,5.37182213056929));
#9805=CARTESIAN_POINT('Ctrl Pts',(-16.4604824035133,-10.8072732748174,5.33477508139295));
#9806=CARTESIAN_POINT('Ctrl Pts',(-16.5955180341857,-10.5629729014716,5.31602326646523));
#9807=CARTESIAN_POINT('Ctrl Pts',(-16.663192795737,-10.2814391939682,5.29727145153752));
#9808=CARTESIAN_POINT('Ctrl Pts',(-16.6632775623115,-9.9999437523457,5.2785196366098));
#9809=CARTESIAN_POINT('Ctrl Pts',(-16.6657318647841,-9.99847819321684,5.47148036339021));
#9810=CARTESIAN_POINT('Ctrl Pts',(-16.661970020417,-10.4143252411811,5.49928516038066));
#9811=CARTESIAN_POINT('Ctrl Pts',(-16.5041909226578,-10.8327185346218,5.52708995737111));
#9812=CARTESIAN_POINT('Ctrl Pts',(-16.2224480983357,-11.1359223423689,5.55489475436156));
#9813=CARTESIAN_POINT('Ctrl Pts',(-15.8470545908295,-11.5399104160786,5.5919418035379));
#9814=CARTESIAN_POINT('Ctrl Pts',(-15.2515902895082,-11.7394044635228,5.62898885271425));
#9815=CARTESIAN_POINT('Ctrl Pts',(-14.7085874340879,-11.6431000067782,5.66603590189058));
#9816=CARTESIAN_POINT('Ctrl Pts',(-14.1655845786677,-11.5467955500336,5.70308295106692));
#9817=CARTESIAN_POINT('Ctrl Pts',(-13.6750431691484,-11.1546925891003,5.74013000024326));
#9818=CARTESIAN_POINT('Ctrl Pts',(-13.461474311529,-10.6462488903663,5.7771770494196));
#9819=CARTESIAN_POINT('Ctrl Pts',(-13.2479054539096,-10.1378051916323,5.81422409859594));
#9820=CARTESIAN_POINT('Ctrl Pts',(-13.3113091481901,-9.51302075509764,5.85127114777229));
#9821=CARTESIAN_POINT('Ctrl Pts',(-13.6226667771701,-9.05784708175693,5.88831819694863));
#9822=CARTESIAN_POINT('Ctrl Pts',(-13.9340244061501,-8.60267340841622,5.92536524612496));
#9823=CARTESIAN_POINT('Ctrl Pts',(-14.4933359698297,-8.31711049826945,5.9624122953013));
#9824=CARTESIAN_POINT('Ctrl Pts',(-15.044615621323,-8.3318548210974,5.99945934447764));
#9825=CARTESIAN_POINT('Ctrl Pts',(-15.5958952728164,-8.34659914392535,6.03650639365398));
#9826=CARTESIAN_POINT('Ctrl Pts',(-16.1391430121236,-8.66165069972803,6.07355344283032));
#9827=CARTESIAN_POINT('Ctrl Pts',(-16.4257250890118,-9.13281667594263,6.11060049200666));
#9828=CARTESIAN_POINT('Ctrl Pts',(-16.582706372449,-9.39090762308494,6.13089378246785));
#9829=CARTESIAN_POINT('Ctrl Pts',(-16.6626744024472,-9.6958411408748,6.15118707292903));
#9830=CARTESIAN_POINT('Ctrl Pts',(-16.6633787344493,-10.0004304228837,6.17148036339021));
#9831=CARTESIAN_POINT('Origin',(-15.,-10.,4.));
#9832=CARTESIAN_POINT('',(-16.6673099838652,-10.001299617498,6.87148036339021));
#9833=CARTESIAN_POINT('',(-16.6681788248613,-9.99913246376521,6.6785196366098));
#9834=CARTESIAN_POINT('',(-16.666,-10.,4.));
#9835=CARTESIAN_POINT('Ctrl Pts',(-16.6681788248613,-9.99913246376521,6.6785196366098));
#9836=CARTESIAN_POINT('Ctrl Pts',(-16.6684949259027,-9.94921615609046,6.67516937498693));
#9837=CARTESIAN_POINT('Ctrl Pts',(-16.6664486628489,-9.89932612429603,6.67181911336406));
#9838=CARTESIAN_POINT('Ctrl Pts',(-16.6619555807564,-9.84965743684369,6.66846885174119));
#9839=CARTESIAN_POINT('Ctrl Pts',(-16.612271271896,-9.30042322360766,6.63142180256485));
#9840=CARTESIAN_POINT('Ctrl Pts',(-16.2633938106262,-8.77825464556249,6.59437475338851));
#9841=CARTESIAN_POINT('Ctrl Pts',(-15.7749977417139,-8.5221375949982,6.55732770421217));
#9842=CARTESIAN_POINT('Ctrl Pts',(-15.2866016728016,-8.26602054443391,6.52028065503583));
#9843=CARTESIAN_POINT('Ctrl Pts',(-14.6586869962468,-8.27595502135049,6.48323360585949));
#9844=CARTESIAN_POINT('Ctrl Pts',(-14.1786377296675,-8.54739438937554,6.44618655668315));
#9845=CARTESIAN_POINT('Ctrl Pts',(-13.6985884630883,-8.8188337574006,6.40913950750681));
#9846=CARTESIAN_POINT('Ctrl Pts',(-13.3664046064846,-9.35177801653412,6.37209245833047));
#9847=CARTESIAN_POINT('Ctrl Pts',(-13.3341202049555,-9.90230902307224,6.33504540915413));
#9848=CARTESIAN_POINT('Ctrl Pts',(-13.3018358034264,-10.4528400296104,6.29799835997779));
#9849=CARTESIAN_POINT('Ctrl Pts',(-13.5694508569717,-11.0209577835531,6.26095131080145));
#9850=CARTESIAN_POINT('Ctrl Pts',(-14.0144832145534,-11.3466460666222,6.22390426162511));
#9851=CARTESIAN_POINT('Ctrl Pts',(-14.4595155721351,-11.6723343496913,6.18685721244877));
#9852=CARTESIAN_POINT('Ctrl Pts',(-15.0819652337531,-11.7555931618868,6.14981016327243));
#9853=CARTESIAN_POINT('Ctrl Pts',(-15.5969493099184,-11.5583165663653,6.11276311409609));
#9854=CARTESIAN_POINT('Ctrl Pts',(-16.1119333860836,-11.3610399708438,6.07571606491975));
#9855=CARTESIAN_POINT('Ctrl Pts',(-16.5194518767962,-10.8832279676053,6.03866901574341));
#9856=CARTESIAN_POINT('Ctrl Pts',(-16.6329916163336,-10.3435656777544,6.00162196656707));
#9857=CARTESIAN_POINT('Ctrl Pts',(-16.6565925290862,-10.2313888956821,5.99392118991465));
#9858=CARTESIAN_POINT('Ctrl Pts',(-16.6674912767693,-10.116539700903,5.98622041326222));
#9859=CARTESIAN_POINT('Ctrl Pts',(-16.6664295714326,-10.0014906689886,5.9785196366098));
#9860=CARTESIAN_POINT('Ctrl Pts',(-16.6633787344493,-10.0004304228837,6.17148036339021));
#9861=CARTESIAN_POINT('Ctrl Pts',(-16.6639602176958,-10.2518936021923,6.18823412210537));
#9862=CARTESIAN_POINT('Ctrl Pts',(-16.610516809841,-10.5031221558014,6.20498788082052));
#9863=CARTESIAN_POINT('Ctrl Pts',(-16.5017821786186,-10.7275639185705,6.22174163953568));
#9864=CARTESIAN_POINT('Ctrl Pts',(-16.2613407768679,-11.2238647883572,6.25878868871202));
#9865=CARTESIAN_POINT('Ctrl Pts',(-15.7505415588973,-11.5891861313041,6.29583573788836));
#9866=CARTESIAN_POINT('Ctrl Pts',(-15.2031672337665,-11.6563278030662,6.3328827870647));
#9867=CARTESIAN_POINT('Ctrl Pts',(-14.6557929086356,-11.7234694748282,6.36992983624104));
#9868=CARTESIAN_POINT('Ctrl Pts',(-14.0718434763445,-11.4924314754053,6.40697688541738));
#9869=CARTESIAN_POINT('Ctrl Pts',(-13.7185810400186,-11.0689549177826,6.44402393459372));
#9870=CARTESIAN_POINT('Ctrl Pts',(-13.3653186036927,-10.64547836016,6.48107098377006));
#9871=CARTESIAN_POINT('Ctrl Pts',(-13.242743163332,-10.0295632443375,6.5181180329464));
#9872=CARTESIAN_POINT('Ctrl Pts',(-13.4069550915532,-9.50310254240692,6.55516508212274));
#9873=CARTESIAN_POINT('Ctrl Pts',(-13.5711670197744,-8.97664184047631,6.59221213129908));
#9874=CARTESIAN_POINT('Ctrl Pts',(-14.0221663165775,-8.53963555243749,6.62925918047543));
#9875=CARTESIAN_POINT('Ctrl Pts',(-14.5535394869087,-8.392091269177,6.66630622965176));
#9876=CARTESIAN_POINT('Ctrl Pts',(-15.0849126572399,-8.24454698591652,6.7033532788281));
#9877=CARTESIAN_POINT('Ctrl Pts',(-15.6966597010992,-8.38646470743436,6.74040032800444));
#9878=CARTESIAN_POINT('Ctrl Pts',(-16.1087961519145,-8.75289449913704,6.77744737718078));
#9879=CARTESIAN_POINT('Ctrl Pts',(-16.4574916805962,-9.06291907883561,6.80879170591726));
#9880=CARTESIAN_POINT('Ctrl Pts',(-16.663299692646,-9.53365643270811,6.84013603465374));
#9881=CARTESIAN_POINT('Ctrl Pts',(-16.6673099838652,-10.001299617498,6.87148036339021));
#9882=CARTESIAN_POINT('Origin',(-15.,-10.,4.));
#9883=CARTESIAN_POINT('',(-16.6674570171079,-9.99879340680734,7.57148036339021));
#9884=CARTESIAN_POINT('',(-16.6638186297495,-9.99906044123799,7.37851963660979));
#9885=CARTESIAN_POINT('',(-16.666,-10.,4.));
#9886=CARTESIAN_POINT('',(-13.7309291201476,-8.9206413469515,8.));
#9887=CARTESIAN_POINT('Ctrl Pts',(-16.6674570171079,-9.99879340680734,7.57148036339021));
#9888=CARTESIAN_POINT('Ctrl Pts',(-16.6635089329096,-10.471496226622,7.60317909473112));
#9889=CARTESIAN_POINT('Ctrl Pts',(-16.4524517931744,-10.947171006763,7.63487782607203));
#9890=CARTESIAN_POINT('Ctrl Pts',(-16.0968414251746,-11.2574592188118,7.66657655741294));
#9891=CARTESIAN_POINT('Ctrl Pts',(-15.6812312656001,-11.6201003140335,7.70362360658928));
#9892=CARTESIAN_POINT('Ctrl Pts',(-15.0681737708883,-11.7568375153793,7.74067065576562));
#9893=CARTESIAN_POINT('Ctrl Pts',(-14.5382154198475,-11.6038879901502,7.77771770494196));
#9894=CARTESIAN_POINT('Ctrl Pts',(-14.0082570688068,-11.4509384649211,7.8147647541183));
#9895=CARTESIAN_POINT('Ctrl Pts',(-13.5613978614371,-11.0083022131172,7.85181180329464));
#9896=CARTESIAN_POINT('Ctrl Pts',(-13.402335136949,-10.4812300903389,7.88885885247098));
#9897=CARTESIAN_POINT('Ctrl Pts',(-13.2432724124609,-9.95415796756067,7.92590590164732));
#9898=CARTESIAN_POINT('Ctrl Pts',(-13.3720061708544,-9.34264997380806,7.96295295082366));
#9899=CARTESIAN_POINT('Ctrl Pts',(-13.7309291201476,-8.92064134695149,8.));
#9900=CARTESIAN_POINT('',(-16.,-8.66750009380863,8.));
#9901=CARTESIAN_POINT('Origin',(-15.,-10.,8.));
#9902=CARTESIAN_POINT('',(-16.2714530003192,-8.91876393899414,8.));
#9903=CARTESIAN_POINT('Origin',(-15.,-10.,8.));
#9904=CARTESIAN_POINT('Ctrl Pts',(-16.2714538290145,-8.91876328587891,8.));
#9905=CARTESIAN_POINT('Ctrl Pts',(-15.9205596240576,-8.50717209253843,7.96367382485347));
#9906=CARTESIAN_POINT('Ctrl Pts',(-15.3505268241097,-8.28122091268906,7.92734764970694));
#9907=CARTESIAN_POINT('Ctrl Pts',(-14.8130932124341,-8.34188937586933,7.89102147456041));
#9908=CARTESIAN_POINT('Ctrl Pts',(-14.2649945105902,-8.40376177310978,7.85397442538407));
#9909=CARTESIAN_POINT('Ctrl Pts',(-13.7508016625205,-8.76374232028908,7.81692737620773));
#9910=CARTESIAN_POINT('Ctrl Pts',(-13.5055195900293,-9.25757781397449,7.77988032703139));
#9911=CARTESIAN_POINT('Ctrl Pts',(-13.2602375175381,-9.75141330765989,7.74283327785505));
#9912=CARTESIAN_POINT('Ctrl Pts',(-13.2838662206256,-10.3791037478514,7.70578622867871));
#9913=CARTESIAN_POINT('Ctrl Pts',(-13.5657615293288,-10.8531100236876,7.66873917950237));
#9914=CARTESIAN_POINT('Ctrl Pts',(-13.8476568380319,-11.3271162995237,7.63169213032602));
#9915=CARTESIAN_POINT('Ctrl Pts',(-14.3878187523508,-11.6474384110046,7.59464508114969));
#9916=CARTESIAN_POINT('Ctrl Pts',(-14.9389380738973,-11.6676039864443,7.55759803197335));
#9917=CARTESIAN_POINT('Ctrl Pts',(-15.4900573954438,-11.6877695618841,7.52055098279701));
#9918=CARTESIAN_POINT('Ctrl Pts',(-16.052134124218,-11.4077786012828,7.48350393362067));
#9919=CARTESIAN_POINT('Ctrl Pts',(-16.3679621297839,-10.9557089721593,7.44645688444433));
#9920=CARTESIAN_POINT('Ctrl Pts',(-16.5610183107237,-10.6793723757226,7.42381113516615));
#9921=CARTESIAN_POINT('Ctrl Pts',(-16.6620634106456,-10.3387384131736,7.40116538588797));
#9922=CARTESIAN_POINT('Ctrl Pts',(-16.6638186297495,-9.99906044123799,7.37851963660979));
#9923=CARTESIAN_POINT('Origin',(15.,-10.,4.));
#9924=CARTESIAN_POINT('',(13.332808903179,-9.99865075154404,0.571480363390208));
#9925=CARTESIAN_POINT('',(13.3364072036082,-9.99933549113491,0.378519636609792));
#9926=CARTESIAN_POINT('',(13.334,-10.,4.));
#9927=CARTESIAN_POINT('',(16.6117095221421,-10.4218393251423,0.));
#9928=CARTESIAN_POINT('Ctrl Pts',(13.3364072036082,-9.99933549113491,0.378519636609792));
#9929=CARTESIAN_POINT('Ctrl Pts',(13.335429121529,-9.77385612213223,0.363487571935548));
#9930=CARTESIAN_POINT('Ctrl Pts',(13.378096681235,-9.54871085704481,0.348455507261303));
#9931=CARTESIAN_POINT('Ctrl Pts',(13.4661893677241,-9.34297029044533,0.333423442587059));
#9932=CARTESIAN_POINT('Ctrl Pts',(13.6832968748538,-8.83591546773436,0.296376393410719));
#9933=CARTESIAN_POINT('Ctrl Pts',(14.1763135429627,-8.44672347685267,0.25932934423438));
#9934=CARTESIAN_POINT('Ctrl Pts',(14.7201521567332,-8.35458602338615,0.222282295058041));
#9935=CARTESIAN_POINT('Ctrl Pts',(15.2639907705037,-8.26244856991963,0.185235245881701));
#9936=CARTESIAN_POINT('Ctrl Pts',(15.8586513299358,-8.46736565386832,0.14818819670536));
#9937=CARTESIAN_POINT('Ctrl Pts',(16.2306499484275,-8.87322647615437,0.111141147529019));
#9938=CARTESIAN_POINT('Ctrl Pts',(16.6026485669192,-9.27908729844041,0.0740940983526795));
#9939=CARTESIAN_POINT('Ctrl Pts',(16.7519852444706,-9.88589185906381,0.0370470491763399));
#9940=CARTESIAN_POINT('Ctrl Pts',(16.6117095221421,-10.4218393251423,0.));
#9941=CARTESIAN_POINT('',(14.324922814325,-11.5230977622533,0.));
#9942=CARTESIAN_POINT('Origin',(15.,-10.,0.));
#9943=CARTESIAN_POINT('Ctrl Pts',(14.3235906297078,-11.5258236994894,2.84494650060196E-15));
#9944=CARTESIAN_POINT('Ctrl Pts',(14.818318071977,-11.7444072143423,0.0363261751465322));
#9945=CARTESIAN_POINT('Ctrl Pts',(15.4299365508059,-11.700654408249,0.0726523502930616));
#9946=CARTESIAN_POINT('Ctrl Pts',(15.8878244848826,-11.4128103339302,0.108978525439591));
#9947=CARTESIAN_POINT('Ctrl Pts',(16.354798966577,-11.1192541438444,0.146025574615931));
#9948=CARTESIAN_POINT('Ctrl Pts',(16.6618809586961,-10.5718228333455,0.18307262379227));
#9949=CARTESIAN_POINT('Ctrl Pts',(16.6686052646603,-10.0204684891763,0.22011967296861));
#9950=CARTESIAN_POINT('Ctrl Pts',(16.6753295706245,-9.46911414500705,0.257166722144951));
#9951=CARTESIAN_POINT('Ctrl Pts',(16.3816961904339,-8.91383676716756,0.294213771321292));
#9952=CARTESIAN_POINT('Ctrl Pts',(15.922053673819,-8.60908166657342,0.331260820497633));
#9953=CARTESIAN_POINT('Ctrl Pts',(15.4624111572042,-8.30432656597928,0.368307869673972));
#9954=CARTESIAN_POINT('Ctrl Pts',(14.8367595041652,-8.25009374263046,0.405354918850311));
#9955=CARTESIAN_POINT('Ctrl Pts',(14.3314686216281,-8.47104689559278,0.44240196802665));
#9956=CARTESIAN_POINT('Ctrl Pts',(13.826177739091,-8.69200004855511,0.47944901720299));
#9957=CARTESIAN_POINT('Ctrl Pts',(13.441247627056,-9.18813917782859,0.51649606637933));
#9958=CARTESIAN_POINT('Ctrl Pts',(13.3528420869761,-9.73247249456812,0.55354311555567));
#9959=CARTESIAN_POINT('Ctrl Pts',(13.3385741752475,-9.8203233205136,0.559522198167183));
#9960=CARTESIAN_POINT('Ctrl Pts',(13.332029912926,-9.90942947246795,0.565501280778695));
#9961=CARTESIAN_POINT('Ctrl Pts',(13.332808903179,-9.99865075154404,0.571480363390208));
#9962=CARTESIAN_POINT('Origin',(15.,-10.,4.));
#9963=CARTESIAN_POINT('',(13.3366507554646,-9.99963522356343,1.27148036339021));
#9964=CARTESIAN_POINT('',(13.3350094287786,-10.0014379681814,1.07851963660979));
#9965=CARTESIAN_POINT('',(13.334,-10.,4.));
#9966=CARTESIAN_POINT('Ctrl Pts',(13.3350094287786,-10.0014379681814,1.07851963660979));
#9967=CARTESIAN_POINT('Ctrl Pts',(13.3382278453089,-9.61090143175114,1.05243653366026));
#9968=CARTESIAN_POINT('Ctrl Pts',(13.4753924362828,-9.21832997108139,1.02635343071072));
#9969=CARTESIAN_POINT('Ctrl Pts',(13.7262226675361,-8.92195568147024,1.00027032776118));
#9970=CARTESIAN_POINT('Ctrl Pts',(14.0824885585281,-8.5010014375266,0.963223278584839));
#9971=CARTESIAN_POINT('Ctrl Pts',(14.6680617783195,-8.27411389904732,0.926176229408499));
#9972=CARTESIAN_POINT('Ctrl Pts',(15.2149469785867,-8.34515454403535,0.889129180232159));
#9973=CARTESIAN_POINT('Ctrl Pts',(15.761832178854,-8.41619518902339,0.852082131055819));
#9974=CARTESIAN_POINT('Ctrl Pts',(16.270029359597,-8.78516401747873,0.815035081879478));
#9975=CARTESIAN_POINT('Ctrl Pts',(16.5069274603671,-9.28315343747998,0.777988032703138));
#9976=CARTESIAN_POINT('Ctrl Pts',(16.7438255611371,-9.78114285748121,0.740940983526799));
#9977=CARTESIAN_POINT('Ctrl Pts',(16.7094245819342,-10.4081528690283,0.703893934350459));
#9978=CARTESIAN_POINT('Ctrl Pts',(16.4195064837655,-10.8772867275589,0.66684688517412));
#9979=CARTESIAN_POINT('Ctrl Pts',(16.1295883855967,-11.3464205860894,0.629799835997779));
#9980=CARTESIAN_POINT('Ctrl Pts',(15.584153168462,-11.6576782916034,0.592752786821439));
#9981=CARTESIAN_POINT('Ctrl Pts',(15.0327634293889,-11.6684612152136,0.555705737645099));
#9982=CARTESIAN_POINT('Ctrl Pts',(14.4813736903159,-11.6792441388238,0.518658688468759));
#9983=CARTESIAN_POINT('Ctrl Pts',(13.9240294293046,-11.3895522805303,0.481611639292419));
#9984=CARTESIAN_POINT('Ctrl Pts',(13.6159564718742,-10.9322475241134,0.444564590116079));
#9985=CARTESIAN_POINT('Ctrl Pts',(13.4328859835592,-10.6604969434577,0.422549605613984));
#9986=CARTESIAN_POINT('Ctrl Pts',(13.3378396390242,-10.3295579137833,0.400534621111888));
#9987=CARTESIAN_POINT('Ctrl Pts',(13.3364072036082,-9.99933549113491,0.378519636609792));
#9988=CARTESIAN_POINT('Ctrl Pts',(13.332808903179,-9.99865075154404,0.571480363390208));
#9989=CARTESIAN_POINT('Ctrl Pts',(13.3368566216514,-10.4622542665498,0.602548329955035));
#9990=CARTESIAN_POINT('Ctrl Pts',(13.5386288752517,-10.9289661622094,0.633616296519862));
#9991=CARTESIAN_POINT('Ctrl Pts',(13.8819529433812,-11.2388249495348,0.664684263084689));
#9992=CARTESIAN_POINT('Ctrl Pts',(14.2913503079907,-11.6083165835564,0.701731312261029));
#9993=CARTESIAN_POINT('Ctrl Pts',(14.9020260053343,-11.7547723473939,0.73877836143737));
#9994=CARTESIAN_POINT('Ctrl Pts',(15.4344828856238,-11.6111839655915,0.77582541061371));
#9995=CARTESIAN_POINT('Ctrl Pts',(15.9669397659133,-11.4675955837891,0.81287245979005));
#9996=CARTESIAN_POINT('Ctrl Pts',(16.4211778291486,-11.0339630563467,0.849919508966388));
#9997=CARTESIAN_POINT('Ctrl Pts',(16.5893028175547,-10.5087402588661,0.886966558142728));
#9998=CARTESIAN_POINT('Ctrl Pts',(16.7574278059609,-9.98351746138546,0.924013607319068));
#9999=CARTESIAN_POINT('Ctrl Pts',(16.6394397195377,-9.36670439386655,0.961060656495409));
#10000=CARTESIAN_POINT('Ctrl Pts',(16.2893385866089,-8.94060996175609,0.99810770567175));
#10001=CARTESIAN_POINT('Ctrl Pts',(15.93923745368,-8.51451552964562,1.03515475484809));
#10002=CARTESIAN_POINT('Ctrl Pts',(15.3570232742455,-8.27913973294359,1.07220180402443));
#10003=CARTESIAN_POINT('Ctrl Pts',(14.8091643748095,-8.34220645059644,1.10924885320077));
#10004=CARTESIAN_POINT('Ctrl Pts',(14.2613054753736,-8.4052731682493,1.14629590237711));
#10005=CARTESIAN_POINT('Ctrl Pts',(13.7478018559363,-8.76678240025705,1.18334295155345));
#10006=CARTESIAN_POINT('Ctrl Pts',(13.5036737629058,-9.26128004979684,1.22039000072979));
#10007=CARTESIAN_POINT('Ctrl Pts',(13.3914507646209,-9.48859517845444,1.2374201216166));
#10008=CARTESIAN_POINT('Ctrl Pts',(13.3361505793704,-9.74401261814188,1.2544502425034));
#10009=CARTESIAN_POINT('Ctrl Pts',(13.3366507554646,-9.99963522356343,1.27148036339021));
#10010=CARTESIAN_POINT('Origin',(15.,-10.,4.));
#10011=CARTESIAN_POINT('',(13.3341441093425,-10.001523795318,1.97148036339021));
#10012=CARTESIAN_POINT('',(13.3312584258872,-9.99997573739076,1.7785196366098));
#10013=CARTESIAN_POINT('',(13.334,-10.,4.));
#10014=CARTESIAN_POINT('Ctrl Pts',(13.3312589065494,-9.99997574164457,1.7785196366098));
#10015=CARTESIAN_POINT('Ctrl Pts',(13.3311402696763,-9.44720220187264,1.74138549538496));
#10016=CARTESIAN_POINT('Ctrl Pts',(13.633172680189,-8.89454120416279,1.70425135416013));
#10017=CARTESIAN_POINT('Ctrl Pts',(14.0982990508631,-8.595851335138,1.6671172129353));
#10018=CARTESIAN_POINT('Ctrl Pts',(14.5623345437871,-8.29786199429832,1.63007016375896));
#10019=CARTESIAN_POINT('Ctrl Pts',(15.1886983610305,-8.25265388018618,1.59302311458262));
#10020=CARTESIAN_POINT('Ctrl Pts',(15.6907163532175,-8.48091822226867,1.55597606540628));
#10021=CARTESIAN_POINT('Ctrl Pts',(16.1927343454045,-8.70918256435115,1.51892901622994));
#10022=CARTESIAN_POINT('Ctrl Pts',(16.5704065125352,-9.21091936262827,1.4818819670536));
#10023=CARTESIAN_POINT('Ctrl Pts',(16.6508794054907,-9.75649288727719,1.44483491787726));
#10024=CARTESIAN_POINT('Ctrl Pts',(16.7313522984462,-10.3020664119261,1.40778786870092));
#10025=CARTESIAN_POINT('Ctrl Pts',(16.5146259172266,-10.8914766629468,1.37074081952458));
#10026=CARTESIAN_POINT('Ctrl Pts',(16.0998923475637,-11.2549636062132,1.33369377034824));
#10027=CARTESIAN_POINT('Ctrl Pts',(15.6851587779009,-11.6184505494795,1.2966467211719));
#10028=CARTESIAN_POINT('Ctrl Pts',(15.072418019795,-11.7560141849915,1.25959967199556));
#10029=CARTESIAN_POINT('Ctrl Pts',(14.5421080391536,-11.6046916700352,1.22255262281922));
#10030=CARTESIAN_POINT('Ctrl Pts',(14.0117980585123,-11.453369155079,1.18550557364288));
#10031=CARTESIAN_POINT('Ctrl Pts',(13.5639188553357,-11.0131604896544,1.14845852446654));
#10032=CARTESIAN_POINT('Ctrl Pts',(13.4034585348436,-10.4855456822382,1.1114114752902));
#10033=CARTESIAN_POINT('Ctrl Pts',(13.3559708572951,-10.3293999025988,1.1004475290634));
#10034=CARTESIAN_POINT('Ctrl Pts',(13.3336565780138,-10.165598712143,1.08948358283659));
#10035=CARTESIAN_POINT('Ctrl Pts',(13.3350094287786,-10.0014379681814,1.07851963660979));
#10036=CARTESIAN_POINT('Ctrl Pts',(13.3366507554646,-9.99963522356343,1.27148036339021));
#10037=CARTESIAN_POINT('Ctrl Pts',(13.3372386543453,-10.3000898941977,1.29149729167974));
#10038=CARTESIAN_POINT('Ctrl Pts',(13.4149162640182,-10.6008280068514,1.31151421996928));
#10039=CARTESIAN_POINT('Ctrl Pts',(13.5678609198539,-10.8565494916407,1.33153114825881));
#10040=CARTESIAN_POINT('Ctrl Pts',(13.8509287364562,-11.3298352168729,1.36857819743515));
#10041=CARTESIAN_POINT('Ctrl Pts',(14.3918169362847,-11.6489206002655,1.40562524661149));
#10042=CARTESIAN_POINT('Ctrl Pts',(14.9429716267943,-11.6677669773384,1.44267229578783));
#10043=CARTESIAN_POINT('Ctrl Pts',(15.4941263173039,-11.6866133544114,1.47971934496417));
#10044=CARTESIAN_POINT('Ctrl Pts',(16.0555474984946,-11.4052207251646,1.51676639414051));
#10045=CARTESIAN_POINT('Ctrl Pts',(16.3702838225975,-10.9523767230522,1.55381344331685));
#10046=CARTESIAN_POINT('Ctrl Pts',(16.6850201467003,-10.4995327209398,1.59086049249319));
#10047=CARTESIAN_POINT('Ctrl Pts',(16.7530716137152,-9.87523734596178,1.62790754166953));
#10048=CARTESIAN_POINT('Ctrl Pts',(16.5432923975969,-9.36521835878357,1.66495459084587));
#10049=CARTESIAN_POINT('Ctrl Pts',(16.3335131814787,-8.85519937160537,1.70200164002221));
#10050=CARTESIAN_POINT('Ctrl Pts',(15.8459032822273,-8.45945677222701,1.73904868919855));
#10051=CARTESIAN_POINT('Ctrl Pts',(15.3036321193532,-8.3591140693806,1.77609573837489));
#10052=CARTESIAN_POINT('Ctrl Pts',(14.761360956479,-8.25877136653418,1.81314278755123));
#10053=CARTESIAN_POINT('Ctrl Pts',(14.1644285299821,-8.45382856021971,1.85018983672757));
#10054=CARTESIAN_POINT('Ctrl Pts',(13.7860390074197,-8.85501185765043,1.88723688590391));
#10055=CARTESIAN_POINT('Ctrl Pts',(13.4992248982105,-9.15910333804621,1.91531804506601));
#10056=CARTESIAN_POINT('Ctrl Pts',(13.3379731658201,-9.58162320501827,1.94339920422811));
#10057=CARTESIAN_POINT('Ctrl Pts',(13.3341441093425,-10.001523795318,1.97148036339021));
#10058=CARTESIAN_POINT('Origin',(15.,-10.,4.));
#10059=CARTESIAN_POINT('',(13.3314909130637,-9.99943625433425,2.67148036339021));
#10060=CARTESIAN_POINT('',(13.3350798878256,-9.99857774548763,2.47851963660979));
#10061=CARTESIAN_POINT('',(13.334,-10.,4.));
#10062=CARTESIAN_POINT('Ctrl Pts',(13.3350798878256,-9.99857774548763,2.47851963660979));
#10063=CARTESIAN_POINT('Ctrl Pts',(13.3337247030062,-9.83179020445009,2.46738150628601));
#10064=CARTESIAN_POINT('Ctrl Pts',(13.3567684529751,-9.66536860128073,2.45624337596222));
#10065=CARTESIAN_POINT('Ctrl Pts',(13.4057542707778,-9.50696974162459,2.44510524563843));
#10066=CARTESIAN_POINT('Ctrl Pts',(13.5686882595461,-8.98011198609755,2.40805819646209));
#10067=CARTESIAN_POINT('Ctrl Pts',(14.0186257820356,-8.54201183282465,2.37101114728576));
#10068=CARTESIAN_POINT('Ctrl Pts',(14.5496393266922,-8.39317905803324,2.33396409810942));
#10069=CARTESIAN_POINT('Ctrl Pts',(15.0806528713488,-8.24434628324183,2.29691704893308));
#10070=CARTESIAN_POINT('Ctrl Pts',(15.6927424381725,-8.38478088693191,2.25986999975674));
#10071=CARTESIAN_POINT('Ctrl Pts',(16.1057667357084,-8.75020873407366,2.2228229505804));
#10072=CARTESIAN_POINT('Ctrl Pts',(16.5187910332443,-9.11563658121541,2.18577590140406));
#10073=CARTESIAN_POINT('Ctrl Pts',(16.7327500614925,-9.70605767180883,2.14872885222772));
#10074=CARTESIAN_POINT('Ctrl Pts',(16.6497189958645,-10.2512479305517,2.11168180305138));
#10075=CARTESIAN_POINT('Ctrl Pts',(16.5666879302365,-10.7964381892946,2.07463475387504));
#10076=CARTESIAN_POINT('Ctrl Pts',(16.1866667707325,-11.296397616187,2.0375877046987));
#10077=CARTESIAN_POINT('Ctrl Pts',(15.6835837031669,-11.5223046908978,2.00054065552236));
#10078=CARTESIAN_POINT('Ctrl Pts',(15.1805006356014,-11.7482117656085,1.96349360634602));
#10079=CARTESIAN_POINT('Ctrl Pts',(14.5543556599743,-11.7000664881376,1.92644655716968));
#10080=CARTESIAN_POINT('Ctrl Pts',(14.0917229282246,-11.3999039494764,1.88939950799334));
#10081=CARTESIAN_POINT('Ctrl Pts',(13.630177776544,-11.100447047862,1.85243955086549));
#10082=CARTESIAN_POINT('Ctrl Pts',(13.3313769869357,-10.550156401746,1.81547959373764));
#10083=CARTESIAN_POINT('Ctrl Pts',(13.3312589065494,-9.99997574164457,1.7785196366098));
#10084=CARTESIAN_POINT('Ctrl Pts',(13.3341441093425,-10.001523795318,1.97148036339021));
#10085=CARTESIAN_POINT('Ctrl Pts',(13.332921549439,-10.1355917120949,1.98044625340445));
#10086=CARTESIAN_POINT('Ctrl Pts',(13.3477471050693,-10.2693926123545,1.98941214341869));
#10087=CARTESIAN_POINT('Ctrl Pts',(13.3796577910855,-10.3989865385901,1.99837803343293));
#10088=CARTESIAN_POINT('Ctrl Pts',(13.5115127159413,-10.9344685209231,2.03542508260927));
#10089=CARTESIAN_POINT('Ctrl Pts',(13.9350691842808,-11.3981230844133,2.07247213178561));
#10090=CARTESIAN_POINT('Ctrl Pts',(14.4564737723188,-11.5777447085202,2.10951918096195));
#10091=CARTESIAN_POINT('Ctrl Pts',(14.9778783603568,-11.757366332627,2.14656623013829));
#10092=CARTESIAN_POINT('Ctrl Pts',(15.5971310680934,-11.6529550173506,2.18361327931463));
#10093=CARTESIAN_POINT('Ctrl Pts',(16.0308121730685,-11.312297753733,2.22066032849097));
#10094=CARTESIAN_POINT('Ctrl Pts',(16.4644932780436,-10.9716404901154,2.25770737766731));
#10095=CARTESIAN_POINT('Ctrl Pts',(16.7126027802573,-10.3947372781565,2.29475442684365));
#10096=CARTESIAN_POINT('Ctrl Pts',(16.661585864872,-9.84562531584823,2.33180147601999));
#10097=CARTESIAN_POINT('Ctrl Pts',(16.6105689494867,-9.29651335353996,2.36884852519633));
#10098=CARTESIAN_POINT('Ctrl Pts',(16.2604256165023,-8.7751926408823,2.40589557437267));
#10099=CARTESIAN_POINT('Ctrl Pts',(15.7714095479698,-8.52026136158418,2.44294262354901));
#10100=CARTESIAN_POINT('Ctrl Pts',(15.2823934794373,-8.26533008228607,2.47998967272535));
#10101=CARTESIAN_POINT('Ctrl Pts',(14.6545046753566,-8.2767882363475,2.51703672190169));
#10102=CARTESIAN_POINT('Ctrl Pts',(14.1751154292343,-8.54939165370295,2.55408377107803));
#10103=CARTESIAN_POINT('Ctrl Pts',(13.6957261831121,-8.8219950710584,2.59113082025437));
#10104=CARTESIAN_POINT('Ctrl Pts',(13.3648364949483,-9.35574375170787,2.62817786943071));
#10105=CARTESIAN_POINT('Ctrl Pts',(13.3338880340578,-9.90635147533067,2.66522491860705));
#10106=CARTESIAN_POINT('Ctrl Pts',(13.3321461374468,-9.93734176370615,2.6673100668681));
#10107=CARTESIAN_POINT('Ctrl Pts',(13.3313544140885,-9.96838545925023,2.66939521512916));
#10108=CARTESIAN_POINT('Ctrl Pts',(13.3314909130637,-9.99943625433425,2.67148036339021));
#10109=CARTESIAN_POINT('Origin',(15.,-10.,4.));
#10110=CARTESIAN_POINT('',(13.335810245754,-9.99883056901517,3.37148036339021));
#10111=CARTESIAN_POINT('',(13.336290211156,-10.0008527825146,3.17851963660979));
#10112=CARTESIAN_POINT('',(13.334,-10.,4.));
#10113=CARTESIAN_POINT('Ctrl Pts',(13.336290211156,-10.0008527825146,3.17851963660979));
#10114=CARTESIAN_POINT('Ctrl Pts',(13.3378338117211,-9.66797335838089,3.15633046801071));
#10115=CARTESIAN_POINT('Ctrl Pts',(13.4345606860051,-9.33426795934119,3.13414129941163));
#10116=CARTESIAN_POINT('Ctrl Pts',(13.6203848998586,-9.06119200316891,3.11195213081255));
#10117=CARTESIAN_POINT('Ctrl Pts',(13.9306371185501,-8.60526422326959,3.07490508163621));
#10118=CARTESIAN_POINT('Ctrl Pts',(14.4892540658804,-8.31834502654515,3.03785803245988));
#10119=CARTESIAN_POINT('Ctrl Pts',(15.0405678077089,-8.33175165747664,3.00081098328354));
#10120=CARTESIAN_POINT('Ctrl Pts',(15.5918815495374,-8.34515828840813,2.9637639341072));
#10121=CARTESIAN_POINT('Ctrl Pts',(16.1358920858641,-8.65889074699554,2.92671688493086));
#10122=CARTESIAN_POINT('Ctrl Pts',(16.4236165482283,-9.12935988890904,2.88966983575452));
#10123=CARTESIAN_POINT('Ctrl Pts',(16.7113410105926,-9.59982903082254,2.85262278657817));
#10124=CARTESIAN_POINT('Ctrl Pts',(16.7427793989944,-10.2270348560621,2.81557573740184));
#10125=CARTESIAN_POINT('Ctrl Pts',(16.5035429844033,-10.7239176567056,2.77852868822549));
#10126=CARTESIAN_POINT('Ctrl Pts',(16.2643065698122,-11.220800457349,2.74148163904916));
#10127=CARTESIAN_POINT('Ctrl Pts',(15.7543953522281,-11.5873602333962,2.70443458987282));
#10128=CARTESIAN_POINT('Ctrl Pts',(15.2071856163145,-11.6558298219649,2.66738754069648));
#10129=CARTESIAN_POINT('Ctrl Pts',(14.6599758804009,-11.7242994105336,2.63034049152014));
#10130=CARTESIAN_POINT('Ctrl Pts',(14.0754676261578,-11.4946788116238,2.5932934423438));
#10131=CARTESIAN_POINT('Ctrl Pts',(13.7211787265599,-11.0720608332783,2.55624639316746));
#10132=CARTESIAN_POINT('Ctrl Pts',(13.4734061629112,-10.7765022085018,2.5303374743149));
#10133=CARTESIAN_POINT('Ctrl Pts',(13.3382322457616,-10.3865499401683,2.50442855546235));
#10134=CARTESIAN_POINT('Ctrl Pts',(13.3350798878256,-9.99857774548763,2.47851963660979));
#10135=CARTESIAN_POINT('Ctrl Pts',(13.3314909130637,-9.99943625433425,2.67148036339021));
#10136=CARTESIAN_POINT('Ctrl Pts',(13.3337796057835,-10.5200682119484,2.7064422643055));
#10137=CARTESIAN_POINT('Ctrl Pts',(13.5970248523073,-11.0426961045957,2.74140416522078));
#10138=CARTESIAN_POINT('Ctrl Pts',(14.0177536614366,-11.3490334538225,2.77636606613607));
#10139=CARTESIAN_POINT('Ctrl Pts',(14.4635749833231,-11.6736409420954,2.81341311531241));
#10140=CARTESIAN_POINT('Ctrl Pts',(15.0862248607134,-11.755389152045,2.85046016448875));
#10141=CARTESIAN_POINT('Ctrl Pts',(15.60072875322,-11.5568635438935,2.88750721366509));
#10142=CARTESIAN_POINT('Ctrl Pts',(16.1152326457267,-11.3583379357421,2.92455426284143));
#10143=CARTESIAN_POINT('Ctrl Pts',(16.5215905533498,-10.8795385094896,2.96160131201776));
#10144=CARTESIAN_POINT('Ctrl Pts',(16.6338204946098,-10.3396022977084,2.99864836119411));
#10145=CARTESIAN_POINT('Ctrl Pts',(16.7460504358698,-9.79966608592732,3.03569541037045));
#10146=CARTESIAN_POINT('Ctrl Pts',(16.5641524107667,-9.19859308861758,3.07274245954679));
#10147=CARTESIAN_POINT('Ctrl Pts',(16.1713775496498,-8.81148253467369,3.10978950872313));
#10148=CARTESIAN_POINT('Ctrl Pts',(15.778602688533,-8.42437198072981,3.14683655789947));
#10149=CARTESIAN_POINT('Ctrl Pts',(15.1749509914024,-8.25122387015177,3.18388360707581));
#10150=CARTESIAN_POINT('Ctrl Pts',(14.6367019071036,-8.37128467038591,3.22093065625215));
#10151=CARTESIAN_POINT('Ctrl Pts',(14.0984528228048,-8.49134547062004,3.25797770542849));
#10152=CARTESIAN_POINT('Ctrl Pts',(13.6256063513377,-8.90461518166635,3.29502475460483));
#10153=CARTESIAN_POINT('Ctrl Pts',(13.4345749755091,-9.42194842625029,3.33207180378117));
#10154=CARTESIAN_POINT('Ctrl Pts',(13.366838844212,-9.60538506029802,3.34520799031751));
#10155=CARTESIAN_POINT('Ctrl Pts',(13.3345347092875,-9.80190537509914,3.35834417685386));
#10156=CARTESIAN_POINT('Ctrl Pts',(13.335810245754,-9.99883056901517,3.37148036339021));
#10157=CARTESIAN_POINT('Origin',(15.,-10.,4.));
#10158=CARTESIAN_POINT('',(13.3357192381005,-10.0012124487014,4.07148036339021));
#10159=CARTESIAN_POINT('',(13.3319678875119,-10.0009660455274,3.8785196366098));
#10160=CARTESIAN_POINT('',(13.334,-10.,4.));
#10161=CARTESIAN_POINT('Ctrl Pts',(13.3319678875119,-10.0009660455274,3.8785196366098));
#10162=CARTESIAN_POINT('Ctrl Pts',(13.3353869932426,-9.50559826735267,3.84527942973542));
#10163=CARTESIAN_POINT('Ctrl Pts',(13.5702060950421,-9.00741586198988,3.81203922286105));
#10164=CARTESIAN_POINT('Ctrl Pts',(13.9562882145892,-8.69793856196637,3.77879901598667));
#10165=CARTESIAN_POINT('Ctrl Pts',(14.3865864772631,-8.35301830330904,3.74175196681034));
#10166=CARTESIAN_POINT('Ctrl Pts',(15.0047785911423,-8.2425012022264,3.704704917634));
#10167=CARTESIAN_POINT('Ctrl Pts',(15.527930246067,-8.41696875119106,3.66765786845766));
#10168=CARTESIAN_POINT('Ctrl Pts',(16.0510819009917,-8.59143630015572,3.63061081928132));
#10169=CARTESIAN_POINT('Ctrl Pts',(16.4791930969619,-9.05088849916767,3.59356377010497));
#10170=CARTESIAN_POINT('Ctrl Pts',(16.616325802445,-9.58504315914936,3.55651672092863));
#10171=CARTESIAN_POINT('Ctrl Pts',(16.7534585079282,-10.1191978191311,3.51946967175229));
#10172=CARTESIAN_POINT('Ctrl Pts',(16.5996127229243,-10.7280549400825,3.48242262257596));
#10173=CARTESIAN_POINT('Ctrl Pts',(16.2252006220181,-11.1329526535695,3.44537557339962));
#10174=CARTESIAN_POINT('Ctrl Pts',(15.850788521112,-11.5378503670565,3.40832852422328));
#10175=CARTESIAN_POINT('Ctrl Pts',(15.2558101043037,-11.7387886730791,3.37128147504693));
#10176=CARTESIAN_POINT('Ctrl Pts',(14.712575231494,-11.6438020811096,3.33423442587059));
#10177=CARTESIAN_POINT('Ctrl Pts',(14.1693403586842,-11.54881548914,3.29718737669425));
#10178=CARTESIAN_POINT('Ctrl Pts',(13.6778490298729,-11.1579039991783,3.26014032751792));
#10179=CARTESIAN_POINT('Ctrl Pts',(13.4630471104936,-10.6499800726604,3.22309327834158));
#10180=CARTESIAN_POINT('Ctrl Pts',(13.3768998643064,-10.4462749676569,3.20823539776431));
#10181=CARTESIAN_POINT('Ctrl Pts',(13.3352566152936,-10.2237490441893,3.19337751718705));
#10182=CARTESIAN_POINT('Ctrl Pts',(13.336290211156,-10.0008527825146,3.17851963660979));
#10183=CARTESIAN_POINT('Ctrl Pts',(13.335810245754,-9.99883056901517,3.37148036339021));
#10184=CARTESIAN_POINT('Ctrl Pts',(13.3381320137313,-10.3572794422137,3.3953912260302));
#10185=CARTESIAN_POINT('Ctrl Pts',(13.4517110307273,-10.717069773939,3.41930208867019));
#10186=CARTESIAN_POINT('Ctrl Pts',(13.6653762209856,-11.0017377389844,3.44321295131018));
#10187=CARTESIAN_POINT('Ctrl Pts',(13.9964251224806,-11.442797029013,3.48026000048652));
#10188=CARTESIAN_POINT('Ctrl Pts',(14.5677392056608,-11.7035188309486,3.51730704966286));
#10189=CARTESIAN_POINT('Ctrl Pts',(15.1178393083377,-11.6645759299679,3.55435409883921));
#10190=CARTESIAN_POINT('Ctrl Pts',(15.6679394110145,-11.6256330289872,3.59140114801555));
#10191=CARTESIAN_POINT('Ctrl Pts',(16.196825533188,-11.2870254250901,3.62844819719189));
#10192=CARTESIAN_POINT('Ctrl Pts',(16.4624369517103,-10.8037271250179,3.66549524636823));
#10193=CARTESIAN_POINT('Ctrl Pts',(16.7280483702325,-10.3204288249458,3.70254229554457));
#10194=CARTESIAN_POINT('Ctrl Pts',(16.7303850851034,-9.69243982869853,3.73958934472091));
#10195=CARTESIAN_POINT('Ctrl Pts',(16.4683776281186,-9.20717828583092,3.77663639389725));
#10196=CARTESIAN_POINT('Ctrl Pts',(16.2063701711338,-8.72191674296332,3.81368344307359));
#10197=CARTESIAN_POINT('Ctrl Pts',(15.6800185422933,-8.37938265347533,3.85073049224993));
#10198=CARTESIAN_POINT('Ctrl Pts',(15.1302234772481,-8.33634709894435,3.88777754142627));
#10199=CARTESIAN_POINT('Ctrl Pts',(14.5804284122028,-8.29331154441336,3.92482459060261));
#10200=CARTESIAN_POINT('Ctrl Pts',(14.0071899109527,-8.54977452483937,3.96187163977895));
#10201=CARTESIAN_POINT('Ctrl Pts',(13.6728679037955,-8.98835800381711,3.99891868895529));
#10202=CARTESIAN_POINT('Ctrl Pts',(13.4545962269312,-9.2746997622177,4.02310591376693));
#10203=CARTESIAN_POINT('Ctrl Pts',(13.338162810448,-9.63867046299276,4.04729313857857));
#10204=CARTESIAN_POINT('Ctrl Pts',(13.3357192381005,-10.0012124487014,4.07148036339021));
#10205=CARTESIAN_POINT('Origin',(15.,-10.,4.));
#10206=CARTESIAN_POINT('',(13.3314357387427,-10.0004924312937,4.77148036339021));
#10207=CARTESIAN_POINT('',(13.3333641526241,-9.99853839723902,4.5785196366098));
#10208=CARTESIAN_POINT('',(13.334,-10.,4.));
#10209=CARTESIAN_POINT('Ctrl Pts',(13.3333641526241,-9.99853839723902,4.5785196366098));
#10210=CARTESIAN_POINT('Ctrl Pts',(13.3323717813096,-9.89034515242106,4.57127544063647));
#10211=CARTESIAN_POINT('Ctrl Pts',(13.3420055133055,-9.78232785263767,4.56403124466314));
#10212=CARTESIAN_POINT('Ctrl Pts',(13.3629080587333,-9.67653708828116,4.55678704868981));
#10213=CARTESIAN_POINT('Ctrl Pts',(13.4698043424929,-9.13551974640515,4.51973999951347));
#10214=CARTESIAN_POINT('Ctrl Pts',(13.8714175336596,-8.6527337027222,4.48269295033713));
#10215=CARTESIAN_POINT('Ctrl Pts',(14.3839372136889,-8.44914058575823,4.44564590116079));
#10216=CARTESIAN_POINT('Ctrl Pts',(14.8964568937183,-8.24554746879426,4.40859885198445));
#10217=CARTESIAN_POINT('Ctrl Pts',(15.5198830626101,-8.32114727854928,4.37155180280811));
#10218=CARTESIAN_POINT('Ctrl Pts',(15.9688858866921,-8.64133947654767,4.33450475363177));
#10219=CARTESIAN_POINT('Ctrl Pts',(16.417888710774,-8.96153167454607,4.29745770445543));
#10220=CARTESIAN_POINT('Ctrl Pts',(16.692468190046,-9.52631626078785,4.26041065527909));
#10221=CARTESIAN_POINT('Ctrl Pts',(16.6669547247066,-10.0772024947589,4.22336360610275));
#10222=CARTESIAN_POINT('Ctrl Pts',(16.6414412593673,-10.62808872873,4.18631655692641));
#10223=CARTESIAN_POINT('Ctrl Pts',(16.3158348494168,-11.1650766104304,4.14926950775008));
#10224=CARTESIAN_POINT('Ctrl Pts',(15.8391591121324,-11.4423974015313,4.11222245857374));
#10225=CARTESIAN_POINT('Ctrl Pts',(15.362483374848,-11.7197181926323,4.0751754093974));
#10226=CARTESIAN_POINT('Ctrl Pts',(14.7347383102298,-11.7373718931338,4.03812836022106));
#10227=CARTESIAN_POINT('Ctrl Pts',(14.2432304251484,-11.4872787532933,4.00108131104471));
#10228=CARTESIAN_POINT('Ctrl Pts',(13.751722540067,-11.2371856134528,3.96403426186837));
#10229=CARTESIAN_POINT('Ctrl Pts',(13.3964518345225,-10.7193456332703,3.92698721269203));
#10230=CARTESIAN_POINT('Ctrl Pts',(13.3400186874845,-10.170763935063,3.88994016351569));
#10231=CARTESIAN_POINT('Ctrl Pts',(13.3342197886207,-10.1143933451982,3.88613332121373));
#10232=CARTESIAN_POINT('Ctrl Pts',(13.3315763136454,-10.0576981537274,3.88232647891176));
#10233=CARTESIAN_POINT('Ctrl Pts',(13.3319678875119,-10.0009660455274,3.8785196366098));
#10234=CARTESIAN_POINT('Ctrl Pts',(13.3357192381005,-10.0012124487014,4.07148036339021));
#10235=CARTESIAN_POINT('Ctrl Pts',(13.3344200435276,-10.1939681822487,4.08434018775491));
#10236=CARTESIAN_POINT('Ctrl Pts',(13.3653437139473,-10.3863200439156,4.09720001211961));
#10237=CARTESIAN_POINT('Ctrl Pts',(13.4303165819644,-10.5663859959084,4.1100598364843));
#10238=CARTESIAN_POINT('Ctrl Pts',(13.6174927803551,-11.0851265314924,4.14710688566065));
#10239=CARTESIAN_POINT('Ctrl Pts',(14.0872506902009,-11.501903625131,4.18415393483699));
#10240=CARTESIAN_POINT('Ctrl Pts',(14.6245914022956,-11.6259666398754,4.22120098401333));
#10241=CARTESIAN_POINT('Ctrl Pts',(15.1619321143903,-11.7500296546197,4.25824803318967));
#10242=CARTESIAN_POINT('Ctrl Pts',(15.7668556287338,-11.5813785904697,4.295295082366));
#10243=CARTESIAN_POINT('Ctrl Pts',(16.162500410882,-11.19720170561,4.33234213154234));
#10244=CARTESIAN_POINT('Ctrl Pts',(16.5581451930302,-10.8130248207503,4.36938918071868));
#10245=CARTESIAN_POINT('Ctrl Pts',(16.7445112429831,-10.2133221151808,4.40643622989503));
#10246=CARTESIAN_POINT('Ctrl Pts',(16.6363025037439,-9.67256566237146,4.44348327907137));
#10247=CARTESIAN_POINT('Ctrl Pts',(16.5280937645046,-9.13180920956211,4.4805303282477));
#10248=CARTESIAN_POINT('Ctrl Pts',(16.1253102360732,-8.64999900951287,4.51757737742404));
#10249=CARTESIAN_POINT('Ctrl Pts',(15.6122979772257,-8.44765006641306,4.55462442660038));
#10250=CARTESIAN_POINT('Ctrl Pts',(15.0992857183783,-8.24530112331325,4.59167147577672));
#10251=CARTESIAN_POINT('Ctrl Pts',(14.4760447291148,-8.32241343716287,4.62871852495306));
#10252=CARTESIAN_POINT('Ctrl Pts',(14.0278200900524,-8.64369422625152,4.6657655741294));
#10253=CARTESIAN_POINT('Ctrl Pts',(13.6014795823874,-8.94928879376472,4.70100383721634));
#10254=CARTESIAN_POINT('Ctrl Pts',(13.3334826207238,-9.47579130585967,4.73624210030328));
#10255=CARTESIAN_POINT('Ctrl Pts',(13.3314357387427,-10.0004924312937,4.77148036339021));
#10256=CARTESIAN_POINT('Origin',(15.,-10.,4.));
#10257=CARTESIAN_POINT('',(13.3342680725317,-9.99847819315956,5.47148036339021));
#10258=CARTESIAN_POINT('',(13.3367226502574,-9.99994375235263,5.2785196366098));
#10259=CARTESIAN_POINT('',(13.334,-10.,4.));
#10260=CARTESIAN_POINT('Ctrl Pts',(13.3367226502574,-9.99994375235263,5.2785196366098));
#10261=CARTESIAN_POINT('Ctrl Pts',(13.3366399476421,-9.72530236931467,5.26022440236118));
#10262=CARTESIAN_POINT('Ctrl Pts',(13.4008958576234,-9.45069741139684,5.24192916811256));
#10263=CARTESIAN_POINT('Ctrl Pts',(13.5297031735473,-9.21074369088521,5.22363393386393));
#10264=CARTESIAN_POINT('Ctrl Pts',(13.7905323546587,-8.72484790168481,5.18658688468759));
#10265=CARTESIAN_POINT('Ctrl Pts',(14.3160512106056,-8.38103770500959,5.14953983551125));
#10266=CARTESIAN_POINT('Ctrl Pts',(14.8657401494705,-8.33666823153406,5.11249278633491));
#10267=CARTESIAN_POINT('Ctrl Pts',(15.4154290883355,-8.29229875805853,5.07544573715857));
#10268=CARTESIAN_POINT('Ctrl Pts',(15.9892881101184,-8.54737000778269,5.03839868798223));
#10269=CARTESIAN_POINT('Ctrl Pts',(16.3246732845184,-8.98514091189926,5.00135163880589));
#10270=CARTESIAN_POINT('Ctrl Pts',(16.6600584589185,-9.42291181601583,4.96430458962955));
#10271=CARTESIAN_POINT('Ctrl Pts',(16.7569697859359,-10.0433823745248,4.92725754045321));
#10272=CARTESIAN_POINT('Ctrl Pts',(16.5710528669398,-10.5625754782171,4.89021049127687));
#10273=CARTESIAN_POINT('Ctrl Pts',(16.3851359479437,-11.0817685819094,4.85316344210053));
#10274=CARTESIAN_POINT('Ctrl Pts',(15.9163907829341,-11.499684230785,4.81611639292419));
#10275=CARTESIAN_POINT('Ctrl Pts',(15.3793527678201,-11.6250506936619,4.77906934374785));
#10276=CARTESIAN_POINT('Ctrl Pts',(14.842314752706,-11.7504171565388,4.74202229457151));
#10277=CARTESIAN_POINT('Ctrl Pts',(14.2369838874874,-11.5832344334171,4.70497524539517));
#10278=CARTESIAN_POINT('Ctrl Pts',(13.8404081430543,-11.2000187518216,4.66792819621883));
#10279=CARTESIAN_POINT('Ctrl Pts',(13.52137899072,-10.8917372298759,4.63812534301582));
#10280=CARTESIAN_POINT('Ctrl Pts',(13.3374467998521,-10.4436488559758,4.60832248981281));
#10281=CARTESIAN_POINT('Ctrl Pts',(13.3333641526241,-9.99853839723902,4.5785196366098));
#10282=CARTESIAN_POINT('Ctrl Pts',(13.3314357387427,-10.0004924312937,4.77148036339021));
#10283=CARTESIAN_POINT('Ctrl Pts',(13.3313306719395,-10.0274254300751,4.77328914947962));
#10284=CARTESIAN_POINT('Ctrl Pts',(13.3319263268189,-10.0543536825872,4.77509793556902));
#10285=CARTESIAN_POINT('Ctrl Pts',(13.3332372565238,-10.0812470687196,4.77690672165842));
#10286=CARTESIAN_POINT('Ctrl Pts',(13.3600873509191,-10.6320698577713,4.81395377083476));
#10287=CARTESIAN_POINT('Ctrl Pts',(13.6869958285712,-11.1682661715471,4.8510008200111));
#10288=CARTESIAN_POINT('Ctrl Pts',(14.1643431415556,-11.444429556671,4.88804786918744));
#10289=CARTESIAN_POINT('Ctrl Pts',(14.6416904545399,-11.7205929417949,4.92509491836378));
#10290=CARTESIAN_POINT('Ctrl Pts',(15.2694766028563,-11.7367233982669,4.96214196754013));
#10291=CARTESIAN_POINT('Ctrl Pts',(15.7603762764363,-11.4854383351005,4.99918901671647));
#10292=CARTESIAN_POINT('Ctrl Pts',(16.2512759500163,-11.2341532719342,5.0362360658928));
#10293=CARTESIAN_POINT('Ctrl Pts',(16.6052891488598,-10.7154526891295,5.07328311506914));
#10294=CARTESIAN_POINT('Ctrl Pts',(16.6603910299587,-10.1667355896657,5.11033016424548));
#10295=CARTESIAN_POINT('Ctrl Pts',(16.7154929110576,-9.61801849020194,5.14737721342182));
#10296=CARTESIAN_POINT('Ctrl Pts',(16.4716834744118,-9.03928487407907,5.18442426259816));
#10297=CARTESIAN_POINT('Ctrl Pts',(16.0405494795664,-8.69540967732856,5.2214713117745));
#10298=CARTESIAN_POINT('Ctrl Pts',(15.6094154847211,-8.35153448057806,5.25851836095084));
#10299=CARTESIAN_POINT('Ctrl Pts',(14.9909569316761,-8.24251770319993,5.29556541012718));
#10300=CARTESIAN_POINT('Ctrl Pts',(14.468230074541,-8.41825416861712,5.33261245930352));
#10301=CARTESIAN_POINT('Ctrl Pts',(13.945503217406,-8.59399063403432,5.36965950847986));
#10302=CARTESIAN_POINT('Ctrl Pts',(13.518508056181,-9.05448034224686,5.40670655765621));
#10303=CARTESIAN_POINT('Ctrl Pts',(13.3826718353368,-9.58896625778836,5.44375360683255));
#10304=CARTESIAN_POINT('Ctrl Pts',(13.3487843156306,-9.72230626005756,5.45299585901843));
#10305=CARTESIAN_POINT('Ctrl Pts',(13.3330176438504,-9.86025156147491,5.46223811120432));
#10306=CARTESIAN_POINT('Ctrl Pts',(13.3342680725317,-9.99847819315956,5.47148036339021));
#10307=CARTESIAN_POINT('Origin',(15.,-10.,4.));
#10308=CARTESIAN_POINT('',(13.3366212029652,-10.0004304228509,6.17148036339021));
#10309=CARTESIAN_POINT('',(13.33357064153,-10.0014906687784,5.9785196366098));
#10310=CARTESIAN_POINT('',(13.334,-10.,4.));
#10311=CARTESIAN_POINT('Ctrl Pts',(13.33357064153,-10.0014906687784,5.9785196366098));
#10312=CARTESIAN_POINT('Ctrl Pts',(13.3376166087855,-9.56305959032262,5.94917336408589));
#10313=CARTESIAN_POINT('Ctrl Pts',(13.5153564139545,-9.12172640784843,5.91982709156197));
#10314=CARTESIAN_POINT('Ctrl Pts',(13.8257421956427,-8.81432850902488,5.89048081903805));
#10315=CARTESIAN_POINT('Ctrl Pts',(14.2175765353692,-8.42626610467219,5.85343376986171));
#10316=CARTESIAN_POINT('Ctrl Pts',(14.8208062262297,-8.25165379552422,5.81638672068537));
#10317=CARTESIAN_POINT('Ctrl Pts',(15.3593449655314,-8.37040818713264,5.77933967150903));
#10318=CARTESIAN_POINT('Ctrl Pts',(15.8978837048331,-8.48916257874107,5.74229262233269));
#10319=CARTESIAN_POINT('Ctrl Pts',(16.371731492576,-8.90128367110589,5.70524557315635));
#10320=CARTESIAN_POINT('Ctrl Pts',(16.5640175621394,-9.41815178528104,5.66819852398002));
#10321=CARTESIAN_POINT('Ctrl Pts',(16.7563036317028,-9.93501989945619,5.63115147480367));
#10322=CARTESIAN_POINT('Ctrl Pts',(16.6670279830868,-10.5566350354417,5.59410442562733));
#10323=CARTESIAN_POINT('Ctrl Pts',(16.3370503164634,-10.9984962344251,5.55705737645099));
#10324=CARTESIAN_POINT('Ctrl Pts',(16.0070726498399,-11.4403574334086,5.52001032727465));
#10325=CARTESIAN_POINT('Ctrl Pts',(15.436392965209,-11.7024646953901,5.48296327809831));
#10326=CARTESIAN_POINT('Ctrl Pts',(14.886200072778,-11.6648567074084,5.44591622892197));
#10327=CARTESIAN_POINT('Ctrl Pts',(14.336007180347,-11.6272487194266,5.40886917974563));
#10328=CARTESIAN_POINT('Ctrl Pts',(13.8063010801158,-11.2899254814817,5.37182213056929));
#10329=CARTESIAN_POINT('Ctrl Pts',(13.5395177831381,-10.8072731716464,5.33477508139295));
#10330=CARTESIAN_POINT('Ctrl Pts',(13.4044821697233,-10.5629728295224,5.31602326646523));
#10331=CARTESIAN_POINT('Ctrl Pts',(13.336807416821,-10.2814391579995,5.29727145153752));
#10332=CARTESIAN_POINT('Ctrl Pts',(13.3367226502574,-9.99994375235263,5.2785196366098));
#10333=CARTESIAN_POINT('Ctrl Pts',(13.3342680725317,-9.99847819315956,5.47148036339021));
#10334=CARTESIAN_POINT('Ctrl Pts',(13.3380299170405,-10.4143252567718,5.49928516038066));
#10335=CARTESIAN_POINT('Ctrl Pts',(13.4958090207374,-10.8327185659559,5.52708995737111));
#10336=CARTESIAN_POINT('Ctrl Pts',(13.7775518556619,-11.135922385114,5.55489475436156));
#10337=CARTESIAN_POINT('Ctrl Pts',(14.1529453772945,-11.5399104740277,5.5919418035379));
#10338=CARTESIAN_POINT('Ctrl Pts',(14.7484097010232,-11.7394045289846,5.62898885271425));
#10339=CARTESIAN_POINT('Ctrl Pts',(15.291412576878,-11.6431000686136,5.66603590189058));
#10340=CARTESIAN_POINT('Ctrl Pts',(15.8344154527327,-11.5467956082426,5.70308295106692));
#10341=CARTESIAN_POINT('Ctrl Pts',(16.3249568807135,-11.1546926325437,5.74013000024326));
#10342=CARTESIAN_POINT('Ctrl Pts',(16.5385257463691,-10.6462489146804,5.7771770494196));
#10343=CARTESIAN_POINT('Ctrl Pts',(16.7520946120246,-10.1378051968171,5.81422409859594));
#10344=CARTESIAN_POINT('Ctrl Pts',(16.688690915355,-9.51302073678948,5.85127114777228));
#10345=CARTESIAN_POINT('Ctrl Pts',(16.3773332746596,-9.05784704631197,5.88831819694862));
#10346=CARTESIAN_POINT('Ctrl Pts',(16.0659756339641,-8.60267335583447,5.92536524612496));
#10347=CARTESIAN_POINT('Ctrl Pts',(15.5066640492429,-8.31711043490708,5.9624122953013));
#10348=CARTESIAN_POINT('Ctrl Pts',(14.9553843770011,-8.33185475830429,5.99945934447764));
#10349=CARTESIAN_POINT('Ctrl Pts',(14.4041047047594,-8.34659908170151,6.03650639365398));
#10350=CARTESIAN_POINT('Ctrl Pts',(13.8608569449971,-8.66165064942335,6.07355344283032));
#10351=CARTESIAN_POINT('Ctrl Pts',(13.5742748573298,-9.13281664334238,6.11060049200666));
#10352=CARTESIAN_POINT('Ctrl Pts',(13.4172935679881,-9.39090760018266,6.13089378246785));
#10353=CARTESIAN_POINT('Ctrl Pts',(13.3373255349887,-9.69584112940636,6.15118707292903));
#10354=CARTESIAN_POINT('Ctrl Pts',(13.3366212029652,-10.0004304228509,6.17148036339021));
#10355=CARTESIAN_POINT('Origin',(15.,-10.,4.));
#10356=CARTESIAN_POINT('',(13.3326899541194,-10.0012996150481,6.87148036339021));
#10357=CARTESIAN_POINT('',(13.331821388128,-9.99913246339926,6.6785196366098));
#10358=CARTESIAN_POINT('',(13.334,-10.,4.));
#10359=CARTESIAN_POINT('Ctrl Pts',(13.331821388128,-9.99913246339926,6.6785196366098));
#10360=CARTESIAN_POINT('Ctrl Pts',(13.3315052870993,-9.9492161620323,6.67516937498693));
#10361=CARTESIAN_POINT('Ctrl Pts',(13.3335515498683,-9.89932613655299,6.67181911336406));
#10362=CARTESIAN_POINT('Ctrl Pts',(13.338044631369,-9.84965745540188,6.66846885174119));
#10363=CARTESIAN_POINT('Ctrl Pts',(13.3877289336859,-9.30042331184456,6.63142180256485));
#10364=CARTESIAN_POINT('Ctrl Pts',(13.7366063508799,-8.77825480177775,6.59437475338851));
#10365=CARTESIAN_POINT('Ctrl Pts',(14.225002357486,-8.52213778422821,6.55732770421217));
#10366=CARTESIAN_POINT('Ctrl Pts',(14.7133983640921,-8.26602076667867,6.52028065503583));
#10367=CARTESIAN_POINT('Ctrl Pts',(15.3413129601104,-8.2759552416464,6.48323360585949));
#10368=CARTESIAN_POINT('Ctrl Pts',(15.8213621652753,-8.54739457482633,6.44618655668316));
#10369=CARTESIAN_POINT('Ctrl Pts',(16.3014113704402,-8.81883390800626,6.40913950750682));
#10370=CARTESIAN_POINT('Ctrl Pts',(16.6335951847516,-9.35177809939841,6.37209245833047));
#10371=CARTESIAN_POINT('Ctrl Pts',(16.6658795821906,-9.90230903566246,6.33504540915413));
#10372=CARTESIAN_POINT('Ctrl Pts',(16.6981639796295,-10.4528399719265,6.29799835997779));
#10373=CARTESIAN_POINT('Ctrl Pts',(16.4305489601959,-11.0209576530625,6.26095131080145));
#10374=CARTESIAN_POINT('Ctrl Pts',(15.9855166594699,-11.3466458944622,6.22390426162511));
#10375=CARTESIAN_POINT('Ctrl Pts',(15.5404843587439,-11.672334135862,6.18685721244877));
#10376=CARTESIAN_POINT('Ctrl Pts',(14.9180347767255,-11.7555929375255,6.14981016327243));
#10377=CARTESIAN_POINT('Ctrl Pts',(14.403050766387,-11.5583163672411,6.11276311409609));
#10378=CARTESIAN_POINT('Ctrl Pts',(13.8880667560485,-11.3610397969568,6.07571606491975));
#10379=CARTESIAN_POINT('Ctrl Pts',(13.48054831739,-10.8832278547246,6.03866901574341));
#10380=CARTESIAN_POINT('Ctrl Pts',(13.3670085923569,-10.3435656338298,6.00162196656707));
#10381=CARTESIAN_POINT('Ctrl Pts',(13.3434076826193,-10.231388866091,5.99392118991465));
#10382=CARTESIAN_POINT('Ctrl Pts',(13.3325089363286,-10.1165396859889,5.98622041326223));
#10383=CARTESIAN_POINT('Ctrl Pts',(13.33357064153,-10.0014906687784,5.9785196366098));
#10384=CARTESIAN_POINT('Ctrl Pts',(13.3366212029652,-10.0004304228509,6.17148036339021));
#10385=CARTESIAN_POINT('Ctrl Pts',(13.336039719701,-10.2518936116005,6.18823412210537));
#10386=CARTESIAN_POINT('Ctrl Pts',(13.389483129569,-10.503122174652,6.20498788082052));
#10387=CARTESIAN_POINT('Ctrl Pts',(13.4982177648784,-10.7275639458888,6.22174163953568));
#10388=CARTESIAN_POINT('Ctrl Pts',(13.7386591756668,-11.2238648344,6.25878868871202));
#10389=CARTESIAN_POINT('Ctrl Pts',(14.2494584128161,-11.5891861913062,6.29583573788837));
#10390=CARTESIAN_POINT('Ctrl Pts',(14.7968327585657,-11.6563278655082,6.33288278706471));
#10391=CARTESIAN_POINT('Ctrl Pts',(15.3442071043154,-11.7234695397102,6.36992983624105));
#10392=CARTESIAN_POINT('Ctrl Pts',(15.9281565586655,-11.4924315312079,6.40697688541738));
#10393=CARTESIAN_POINT('Ctrl Pts',(16.2814190082463,-11.0689549578054,6.44402393459372));
#10394=CARTESIAN_POINT('Ctrl Pts',(16.6346814578271,-10.6454783844028,6.48107098377006));
#10395=CARTESIAN_POINT('Ctrl Pts',(16.7572569026387,-10.0295632461,6.5181180329464));
#10396=CARTESIAN_POINT('Ctrl Pts',(16.5930449683129,-9.50310252407789,6.55516508212274));
#10397=CARTESIAN_POINT('Ctrl Pts',(16.4288330339871,-8.97664180205576,6.59221213129908));
#10398=CARTESIAN_POINT('Ctrl Pts',(15.9778337205239,-8.53963549631433,6.62925918047542));
#10399=CARTESIAN_POINT('Ctrl Pts',(15.4464605300519,-8.39209120799975,6.66630622965176));
#10400=CARTESIAN_POINT('Ctrl Pts',(14.9150873395799,-8.24454691968518,6.7033532788281));
#10401=CARTESIAN_POINT('Ctrl Pts',(14.303340272099,-8.38646464879746,6.74040032800445));
#10402=CARTESIAN_POINT('Ctrl Pts',(13.8912038060524,-8.75289445340972,6.77744737718078));
#10403=CARTESIAN_POINT('Ctrl Pts',(13.5425082644839,-9.06291904403068,6.80879170591726));
#10404=CARTESIAN_POINT('Ctrl Pts',(13.3367002455534,-9.53365641263032,6.84013603465373));
#10405=CARTESIAN_POINT('Ctrl Pts',(13.3326899541194,-10.0012996150481,6.87148036339021));
#10406=CARTESIAN_POINT('Origin',(15.,-10.,4.));
#10407=CARTESIAN_POINT('',(13.3325429336747,-9.99879337075124,7.57148036339021));
#10408=CARTESIAN_POINT('',(13.3361815844527,-9.99906045492932,7.3785196366098));
#10409=CARTESIAN_POINT('',(13.334,-10.,4.));
#10410=CARTESIAN_POINT('',(16.2690708798524,-8.9206413469515,8.));
#10411=CARTESIAN_POINT('Ctrl Pts',(13.3325429336747,-9.99879337075124,7.57148036339021));
#10412=CARTESIAN_POINT('Ctrl Pts',(13.3364909776232,-10.4714962597792,7.60317909473112));
#10413=CARTESIAN_POINT('Ctrl Pts',(13.5475480484014,-10.9471711688739,7.63487782607203));
#10414=CARTESIAN_POINT('Ctrl Pts',(13.9031584757476,-11.2574593537338,7.66657655741294));
#10415=CARTESIAN_POINT('Ctrl Pts',(14.3187687046815,-11.6201004171794,7.70362360658928));
#10416=CARTESIAN_POINT('Ctrl Pts',(14.931826444004,-11.7568373734716,7.74067065576562));
#10417=CARTESIAN_POINT('Ctrl Pts',(15.4617847126295,-11.603887923119,7.77771770494196));
#10418=CARTESIAN_POINT('Ctrl Pts',(15.9917429812551,-11.4509384727664,7.8147647541183));
#10419=CARTESIAN_POINT('Ctrl Pts',(16.4386017791837,-11.008302615769,7.85181180329464));
#10420=CARTESIAN_POINT('Ctrl Pts',(16.5976644911563,-10.4812304910294,7.88885885247098));
#10421=CARTESIAN_POINT('Ctrl Pts',(16.756727203129,-9.95415836628982,7.92590590164732));
#10422=CARTESIAN_POINT('Ctrl Pts',(16.6279938291456,-9.34264997380806,7.96295295082366));
#10423=CARTESIAN_POINT('Ctrl Pts',(16.2690708798524,-8.92064134695149,8.));
#10424=CARTESIAN_POINT('',(16.,-8.66750009380863,8.));
#10425=CARTESIAN_POINT('Origin',(15.,-10.,8.));
#10426=CARTESIAN_POINT('',(13.7285472376402,-8.91876346821723,8.));
#10427=CARTESIAN_POINT('Origin',(15.,-10.,8.));
#10428=CARTESIAN_POINT('Ctrl Pts',(13.7285464165792,-8.9187628208919,8.));
#10429=CARTESIAN_POINT('Ctrl Pts',(14.0794406943795,-8.50717132356286,7.96367382485347));
#10430=CARTESIAN_POINT('Ctrl Pts',(14.6494732896009,-8.28122126317251,7.92734764970694));
#10431=CARTESIAN_POINT('Ctrl Pts',(15.1869067713614,-8.34188994522698,7.89102147456041));
#10432=CARTESIAN_POINT('Ctrl Pts',(15.735005340712,-8.40376256568508,7.85397442538407));
#10433=CARTESIAN_POINT('Ctrl Pts',(16.2491981340985,-8.76374239939929,7.81692737620773));
#10434=CARTESIAN_POINT('Ctrl Pts',(16.4944801949704,-9.25757769375947,7.77988032703139));
#10435=CARTESIAN_POINT('Ctrl Pts',(16.7397622558424,-9.75141298811966,7.74283327785505));
#10436=CARTESIAN_POINT('Ctrl Pts',(16.7161335841998,-10.3791037431258,7.70578622867871));
#10437=CARTESIAN_POINT('Ctrl Pts',(16.4342383093536,-10.8531100403582,7.66873917950237));
#10438=CARTESIAN_POINT('Ctrl Pts',(16.1523430345073,-11.3271163375905,7.63169213032603));
#10439=CARTESIAN_POINT('Ctrl Pts',(15.6121811564573,-11.6474381770491,7.59464508114969));
#10440=CARTESIAN_POINT('Ctrl Pts',(15.0610619021163,-11.6676037010972,7.55759803197335));
#10441=CARTESIAN_POINT('Ctrl Pts',(14.5099426477752,-11.6877692251453,7.52055098279701));
#10442=CARTESIAN_POINT('Ctrl Pts',(13.9478660171431,-11.407778433783,7.48350393362067));
#10443=CARTESIAN_POINT('Ctrl Pts',(13.6320380558773,-10.9557088910527,7.44645688444433));
#10444=CARTESIAN_POINT('Ctrl Pts',(13.4389819020169,-10.6793723474257,7.42381113516615));
#10445=CARTESIAN_POINT('Ctrl Pts',(13.3379368090562,-10.3387384067309,7.40116538588797));
#10446=CARTESIAN_POINT('Ctrl Pts',(13.3361815844527,-9.99906045492932,7.3785196366098));
#10447=CARTESIAN_POINT('Origin',(15.,-10.,9.54592528053767));
#10448=CARTESIAN_POINT('',(12.9482189085318,-9.99918043241852,0.154074719462319));
#10449=CARTESIAN_POINT('',(12.9434420405202,-10.0015653531237,0.0959252805376758));
#10450=CARTESIAN_POINT('',(12.94525,-9.99999999999991,9.54592528053767));
#10451=CARTESIAN_POINT('',(13.6609982804014,-8.44145197141315,1.11022302462516E-15));
#10452=CARTESIAN_POINT('Ctrl Pts',(12.9434420405202,-10.0015653531237,0.0959252805376757));
#10453=CARTESIAN_POINT('Ctrl Pts',(12.948189590265,-9.4149504982262,0.0639501870251168));
#10454=CARTESIAN_POINT('Ctrl Pts',(13.2136828890534,-8.82575586659749,0.0319750935125577));
#10455=CARTESIAN_POINT('Ctrl Pts',(13.6609982804014,-8.44145197141313,-1.11022302462516E-15));
#10456=CARTESIAN_POINT('',(14.6157705213662,-7.97768900275326,1.06453246059332E-15));
#10457=CARTESIAN_POINT('Origin',(15.,-10.,0.));
#10458=CARTESIAN_POINT('Ctrl Pts',(12.9482189085318,-9.99918043241852,0.154074719462319));
#10459=CARTESIAN_POINT('Ctrl Pts',(12.947012597516,-9.72108695495263,0.139042654788076));
#10460=CARTESIAN_POINT('Ctrl Pts',(13.1268058099709,-8.77236641039839,0.0876844149673037));
#10461=CARTESIAN_POINT('Ctrl Pts',(13.9605770103796,-8.10301207949468,0.0363261751465313));
#10462=CARTESIAN_POINT('Ctrl Pts',(14.615770327818,-7.97768772784116,8.78610335527941E-16));
#10463=CARTESIAN_POINT('Origin',(15.,-10.,9.54592528053767));
#10464=CARTESIAN_POINT('',(12.9464949722586,-10.0017735084758,0.854074719462319));
#10465=CARTESIAN_POINT('',(12.9437809686717,-9.99833591340643,0.795925280537676));
#10466=CARTESIAN_POINT('',(12.94525,-9.99999999999991,9.54592528053767));
#10467=CARTESIAN_POINT('Ctrl Pts',(12.9437809686717,-9.99833591340643,0.795925280537676));
#10468=CARTESIAN_POINT('Ctrl Pts',(12.9428202062333,-9.88829544330943,0.789946197926164));
#10469=CARTESIAN_POINT('Ctrl Pts',(13.0009023236625,-9.09745398140138,0.746920066138311));
#10470=CARTESIAN_POINT('Ctrl Pts',(14.0270251243106,-7.77487708517042,0.666846885174118));
#10471=CARTESIAN_POINT('Ctrl Pts',(16.3419550176155,-7.97554015919684,0.555705737645099));
#10472=CARTESIAN_POINT('Ctrl Pts',(17.4284073368472,-10.0300831221902,0.444564590116078));
#10473=CARTESIAN_POINT('Ctrl Pts',(16.2921947498604,-12.0555954005474,0.333423442587058));
#10474=CARTESIAN_POINT('Ctrl Pts',(13.9727681426279,-12.2024165492448,0.222282295058038));
#10475=CARTESIAN_POINT('Ctrl Pts',(12.9909165518555,-10.866791374719,0.143116241041578));
#10476=CARTESIAN_POINT('Ctrl Pts',(12.9426889743311,-10.0946154183123,0.100997236201457));
#10477=CARTESIAN_POINT('Ctrl Pts',(12.9434420405202,-10.0015653531237,0.0959252805376757));
#10478=CARTESIAN_POINT('Ctrl Pts',(12.9464949722586,-10.0017735084758,0.854074719462319));
#10479=CARTESIAN_POINT('Ctrl Pts',(12.950464384843,-9.52010787328362,0.827991616512784));
#10480=CARTESIAN_POINT('Ctrl Pts',(13.3599169395246,-8.34823555313923,0.764861464386909));
#10481=CARTESIAN_POINT('Ctrl Pts',(15.3128190350351,-7.59155964248331,0.664684263084691));
#10482=CARTESIAN_POINT('Ctrl Pts',(17.1931638558005,-8.95675538126231,0.553543115555674));
#10483=CARTESIAN_POINT('Ctrl Pts',(17.0658792003075,-11.2767112418142,0.442401968026652));
#10484=CARTESIAN_POINT('Ctrl Pts',(15.0477525273048,-12.4283740936836,0.331260820497633));
#10485=CARTESIAN_POINT('Ctrl Pts',(13.2644774636808,-11.5014779126907,0.235151737642855));
#10486=CARTESIAN_POINT('Ctrl Pts',(12.9499855932083,-10.4064580572305,0.176089703964416));
#10487=CARTESIAN_POINT('Ctrl Pts',(12.9482189085318,-9.99918043241852,0.154074719462319));
#10488=CARTESIAN_POINT('Origin',(15.,-10.,9.54592528053767));
#10489=CARTESIAN_POINT('',(12.9418692906557,-9.99997008111884,1.55407471946232));
#10490=CARTESIAN_POINT('',(12.9485192915911,-9.99955010541237,1.49592528053768));
#10491=CARTESIAN_POINT('',(12.94525,-9.99999999999991,9.54592528053767));
#10492=CARTESIAN_POINT('Ctrl Pts',(12.9485192915911,-9.99955010541237,1.49592528053768));
#10493=CARTESIAN_POINT('Ctrl Pts',(12.9479024027379,-9.68427966814349,1.47889515965087));
#10494=CARTESIAN_POINT('Ctrl Pts',(13.1644766450531,-8.68397852586288,1.42481798958772));
#10495=CARTESIAN_POINT('Ctrl Pts',(14.7222622974566,-7.58728928450919,1.33369377034824));
#10496=CARTESIAN_POINT('Ctrl Pts',(16.8764722347793,-8.45818679640628,1.22255262281922));
#10497=CARTESIAN_POINT('Ctrl Pts',(17.3130316956038,-10.7404136580229,1.1114114752902));
#10498=CARTESIAN_POINT('Ctrl Pts',(15.632337229038,-12.3448670237413,1.00027032776118));
#10499=CARTESIAN_POINT('Ctrl Pts',(13.4943745863678,-11.8321285059805,0.89510826284367));
#10500=CARTESIAN_POINT('Ctrl Pts',(12.948773195281,-10.5701182198038,0.826993247102503));
#10501=CARTESIAN_POINT('Ctrl Pts',(12.9437809686717,-9.99833591340643,0.795925280537676));
#10502=CARTESIAN_POINT('Ctrl Pts',(12.9418692906557,-9.99997008111884,1.55407471946232));
#10503=CARTESIAN_POINT('Ctrl Pts',(12.9418689474861,-9.99837112568582,1.55398762741383));
#10504=CARTESIAN_POINT('Ctrl Pts',(12.9425947611461,-9.31661188450496,1.516853486189));
#10505=CARTESIAN_POINT('Ctrl Pts',(13.6876865848533,-7.95643655777695,1.44267229578783));
#10506=CARTESIAN_POINT('Ctrl Pts',(16.0052515070878,-7.78916517877589,1.33153114825881));
#10507=CARTESIAN_POINT('Ctrl Pts',(17.4026498601701,-9.64560639052843,1.22039000072979));
#10508=CARTESIAN_POINT('Ctrl Pts',(16.6007557452642,-11.8264420086883,1.10924885320077));
#10509=CARTESIAN_POINT('Ctrl Pts',(14.3335965506935,-12.3354315886432,0.998107705671752));
#10510=CARTESIAN_POINT('Ctrl Pts',(13.0653413219675,-11.0888969478397,0.913049661092266));
#10511=CARTESIAN_POINT('Ctrl Pts',(12.9448264427814,-10.2042400682928,0.865038665689123));
#10512=CARTESIAN_POINT('Ctrl Pts',(12.9464949722586,-10.0017735084758,0.854074719462319));
#10513=CARTESIAN_POINT('Origin',(15.,-10.,9.54592528053767));
#10514=CARTESIAN_POINT('',(12.9465818724548,-9.99824587187305,2.25407471946232));
#10515=CARTESIAN_POINT('',(12.9454277362974,-10.001879362803,2.19592528053768));
#10516=CARTESIAN_POINT('',(12.94525,-9.99999999999991,9.54592528053767));
#10517=CARTESIAN_POINT('Ctrl Pts',(12.9454277362974,-10.001879362803,2.19592528053768));
#10518=CARTESIAN_POINT('Ctrl Pts',(12.9501502775923,-9.48399776741373,2.16784412137558));
#10519=CARTESIAN_POINT('Ctrl Pts',(13.4114067583102,-8.27539043040156,2.10271591303714));
#10520=CARTESIAN_POINT('Ctrl Pts',(15.4418987567046,-7.61189477590683,2.00054065552236));
#10521=CARTESIAN_POINT('Ctrl Pts',(17.2460700180853,-9.07615427063553,1.88939950799333));
#10522=CARTESIAN_POINT('Ctrl Pts',(16.9942775477693,-11.3860658944101,1.77825836046432));
#10523=CARTESIAN_POINT('Ctrl Pts',(14.9170023279882,-12.42722706778,1.6671172129353));
#10524=CARTESIAN_POINT('Ctrl Pts',(13.2223586797308,-11.4275084228001,1.57300618629309));
#10525=CARTESIAN_POINT('Ctrl Pts',(12.9492443727587,-10.3701138716103,1.51594220882721));
#10526=CARTESIAN_POINT('Ctrl Pts',(12.9485192915911,-9.99955010541237,1.49592528053768));
#10527=CARTESIAN_POINT('Ctrl Pts',(12.9465818724548,-9.99824587187305,2.25407471946232));
#10528=CARTESIAN_POINT('Ctrl Pts',(12.9449104642869,-9.79253956938397,2.24293658913854));
#10529=CARTESIAN_POINT('Ctrl Pts',(13.067863238549,-8.90457654972051,2.19475140963841));
#10530=CARTESIAN_POINT('Ctrl Pts',(14.3445560924207,-7.66147210297657,2.10951918096195));
#10531=CARTESIAN_POINT('Ctrl Pts',(16.6093058597035,-8.18108435135386,1.99837803343293));
#10532=CARTESIAN_POINT('Ctrl Pts',(17.4009606855609,-10.3656601062701,1.88723688590391));
#10533=CARTESIAN_POINT('Ctrl Pts',(15.9948709901991,-12.2155249905566,1.77609573837489));
#10534=CARTESIAN_POINT('Ctrl Pts',(13.6799312363543,-12.0375256116339,1.66504168289436));
#10535=CARTESIAN_POINT('Ctrl Pts',(12.9420149243134,-10.6785317325855,1.59103467659017));
#10536=CARTESIAN_POINT('Ctrl Pts',(12.9418692906557,-9.99997008111884,1.55407471946232));
#10537=CARTESIAN_POINT('Origin',(15.,-10.,9.54592528053767));
#10538=CARTESIAN_POINT('',(12.9480746166703,-10.0010517736324,2.95407471946232));
#10539=CARTESIAN_POINT('',(12.9421554343443,-9.9993047080392,2.89592528053767));
#10540=CARTESIAN_POINT('',(12.94525,-9.99999999999991,9.54592528053767));
#10541=CARTESIAN_POINT('Ctrl Pts',(12.9421554343443,-9.9993047080392,2.89592528053768));
#10542=CARTESIAN_POINT('Ctrl Pts',(12.9419870842427,-9.96100841680338,2.89384013227662));
#10543=CARTESIAN_POINT('Ctrl Pts',(12.9603125383811,-9.24246220617618,2.85470793483923));
#10544=CARTESIAN_POINT('Ctrl Pts',(13.7994831701705,-7.88882009045181,2.7785286882255));
#10545=CARTESIAN_POINT('Ctrl Pts',(16.122690589471,-7.84642457654237,2.66738754069648));
#10546=CARTESIAN_POINT('Ctrl Pts',(17.4182314300163,-9.77532685925541,2.55624639316745));
#10547=CARTESIAN_POINT('Ctrl Pts',(16.5002188255622,-11.9098860575253,2.44510524563844));
#10548=CARTESIAN_POINT('Ctrl Pts',(14.2089652219215,-12.2962110576408,2.33396409810941));
#10549=CARTESIAN_POINT('Ctrl Pts',(13.0377585044605,-11.0141261883668,2.2509041097425));
#10550=CARTESIAN_POINT('Ctrl Pts',(12.9439199001859,-10.1672311347101,2.20489117055192));
#10551=CARTESIAN_POINT('Ctrl Pts',(12.9454277362974,-10.001879362803,2.19592528053768));
#10552=CARTESIAN_POINT('Ctrl Pts',(12.9480746166703,-10.0010517736324,2.95407471946232));
#10553=CARTESIAN_POINT('Ctrl Pts',(12.9499784061428,-9.59049715374129,2.93188555086324));
#10554=CARTESIAN_POINT('Ctrl Pts',(13.2684549392389,-8.4917607441522,2.87264933308783));
#10555=CARTESIAN_POINT('Ctrl Pts',(15.0590413951949,-7.57207216315973,2.77636606613607));
#10556=CARTESIAN_POINT('Ctrl Pts',(17.0718967064505,-8.73289167567321,2.66522491860705));
#10557=CARTESIAN_POINT('Ctrl Pts',(17.1882196870663,-11.053572052764,2.55408377107803));
#10558=CARTESIAN_POINT('Ctrl Pts',(15.3015328785473,-12.4098542253325,2.44294262354901));
#10559=CARTESIAN_POINT('Ctrl Pts',(13.3555719234122,-11.6453950124307,2.34293960634377));
#10560=CARTESIAN_POINT('Ctrl Pts',(12.950469812112,-10.4767487932537,2.27998363831488));
#10561=CARTESIAN_POINT('Ctrl Pts',(12.9465818724548,-9.99824587187305,2.25407471946232));
#10562=CARTESIAN_POINT('Origin',(15.,-10.,9.54592528053767));
#10563=CARTESIAN_POINT('',(12.9427437076021,-10.0011914658147,3.65407471946232));
#10564=CARTESIAN_POINT('',(12.9474826545396,-9.9985576900864,3.59592528053768));
#10565=CARTESIAN_POINT('',(12.94525,-9.99999999999991,9.54592528053767));
#10566=CARTESIAN_POINT('Ctrl Pts',(12.9474826545396,-9.9985576900864,3.59592528053768));
#10567=CARTESIAN_POINT('Ctrl Pts',(12.9459094801371,-9.75568131421667,3.58278909400133));
#10568=CARTESIAN_POINT('Ctrl Pts',(13.0981153708669,-8.82974568304574,3.53260585828864));
#10569=CARTESIAN_POINT('Ctrl Pts',(14.4712648408794,-7.62960754320777,3.44537557339961));
#10570=CARTESIAN_POINT('Ctrl Pts',(16.7047942370601,-8.27026074886842,3.3342344258706));
#10571=CARTESIAN_POINT('Ctrl Pts',(17.3778223890662,-10.4942488783201,3.22309327834157));
#10572=CARTESIAN_POINT('Ctrl Pts',(15.8742859352451,-12.2658211251852,3.11195213081256));
#10573=CARTESIAN_POINT('Ctrl Pts',(13.6136853347311,-11.9690250296368,3.00289613154459));
#10574=CARTESIAN_POINT('Ctrl Pts',(12.9449781782615,-10.6414226641662,2.93088718145296));
#10575=CARTESIAN_POINT('Ctrl Pts',(12.9421554343443,-9.9993047080392,2.89592528053768));
#10576=CARTESIAN_POINT('Ctrl Pts',(12.9427437076021,-10.0011914658147,3.65407471946232));
#10577=CARTESIAN_POINT('Ctrl Pts',(12.9469606388747,-9.39023291707249,3.62083451258795));
#10578=CARTESIAN_POINT('Ctrl Pts',(13.5593537346582,-8.09100528547459,3.55054725653724));
#10579=CARTESIAN_POINT('Ctrl Pts',(15.7683367683932,-7.69609503710994,3.44321295131019));
#10580=CARTESIAN_POINT('Ctrl Pts',(17.3523610419581,-9.39608196253575,3.33207180378117));
#10581=CARTESIAN_POINT('Ctrl Pts',(16.7831270202232,-11.6488715830789,3.22093065625215));
#10582=CARTESIAN_POINT('Ctrl Pts',(14.5816890215374,-12.3923493459239,3.10978950872313));
#10583=CARTESIAN_POINT('Ctrl Pts',(13.1262237587042,-11.234733613704,3.02083752979318));
#10584=CARTESIAN_POINT('Ctrl Pts',(12.9467998380999,-10.2759593928858,2.96893260003958));
#10585=CARTESIAN_POINT('Ctrl Pts',(12.9480746166703,-10.0010517736324,2.95407471946232));
#10586=CARTESIAN_POINT('Origin',(15.,-10.,9.54592528053767));
#10587=CARTESIAN_POINT('',(12.9444657818754,-9.9981973419728,4.35407471946232));
#10588=CARTESIAN_POINT('',(12.9473704108566,-10.0014953655277,4.29592528053768));
#10589=CARTESIAN_POINT('',(12.94525,-9.99999999999991,9.54592528053767));
#10590=CARTESIAN_POINT('Ctrl Pts',(12.9473704108566,-10.0014953655277,4.29592528053768));
#10591=CARTESIAN_POINT('Ctrl Pts',(12.9503841745306,-9.5543566229498,4.27173805572604));
#10592=CARTESIAN_POINT('Ctrl Pts',(13.3139392105709,-8.41788407722688,4.21050378173806));
#10593=CARTESIAN_POINT('Ctrl Pts',(15.1895240638759,-7.57876025621427,4.11222245857373));
#10594=CARTESIAN_POINT('Ctrl Pts',(17.1370408874533,-8.84614666745458,4.00108131104471));
#10595=CARTESIAN_POINT('Ctrl Pts',(17.1283949723014,-11.1697248007781,3.8899401635157));
#10596=CARTESIAN_POINT('Ctrl Pts',(15.1715004473266,-12.4225830974903,3.77879901598667));
#10597=CARTESIAN_POINT('Ctrl Pts',(13.3074684623944,-11.5719235526181,3.680794054994));
#10598=CARTESIAN_POINT('Ctrl Pts',(12.9503461916053,-10.4406482196211,3.61983614317767));
#10599=CARTESIAN_POINT('Ctrl Pts',(12.9474826545396,-9.9985576900864,3.59592528053768));
#10600=CARTESIAN_POINT('Ctrl Pts',(12.9444657818754,-9.9981973419728,4.35407471946232));
#10601=CARTESIAN_POINT('Ctrl Pts',(12.9432418473265,-9.86475792433196,4.346830523489));
#10602=CARTESIAN_POINT('Ctrl Pts',(13.0158869348842,-9.0502318191971,4.30253927833933));
#10603=CARTESIAN_POINT('Ctrl Pts',(14.1033972880174,-7.74291713830186,4.22120098401333));
#10604=CARTESIAN_POINT('Ctrl Pts',(16.4100928231865,-8.02263870329727,4.1100598364843));
#10605=CARTESIAN_POINT('Ctrl Pts',(17.4260451371735,-10.1123586227095,3.99891868895528));
#10606=CARTESIAN_POINT('Ctrl Pts',(16.2212916482552,-12.0992299010838,3.88777754142627));
#10607=CARTESIAN_POINT('Ctrl Pts',(13.8986160692799,-12.1645491227624,3.77663639389725));
#10608=CARTESIAN_POINT('Ctrl Pts',(12.9772494572038,-10.8215718924642,3.6987354532426));
#10609=CARTESIAN_POINT('Ctrl Pts',(12.9422607625827,-10.0711616334762,3.65788156176429));
#10610=CARTESIAN_POINT('Ctrl Pts',(12.9427437076021,-10.0011914658147,3.65407471946232));
#10611=CARTESIAN_POINT('Origin',(15.,-10.,9.54592528053767));
#10612=CARTESIAN_POINT('',(12.9486079625549,-9.99993062733875,5.05407471946232));
#10613=CARTESIAN_POINT('',(12.9420873854632,-10.0006073368552,4.99592528053768));
#10614=CARTESIAN_POINT('',(12.94525,-9.99999999999991,9.54592528053767));
#10615=CARTESIAN_POINT('Ctrl Pts',(12.9420873854632,-10.0006073368552,4.99592528053768));
#10616=CARTESIAN_POINT('Ctrl Pts',(12.9446118937168,-9.353470699709,4.96068701745075));
#10617=CARTESIAN_POINT('Ctrl Pts',(13.6226427058774,-8.02142229265111,4.88840170518746));
#10618=CARTESIAN_POINT('Ctrl Pts',(15.8911235009165,-7.74074787289641,4.77906934374785));
#10619=CARTESIAN_POINT('Ctrl Pts',(17.381434644454,-9.52346007316861,4.66792819621884));
#10620=CARTESIAN_POINT('Ctrl Pts',(16.6918746664094,-11.7423780820561,4.55678704868981));
#10621=CARTESIAN_POINT('Ctrl Pts',(14.453639508371,-12.3663920809676,4.4456459011608));
#10622=CARTESIAN_POINT('Ctrl Pts',(13.0937812261127,-11.1599030133838,4.35869197844341));
#10623=CARTESIAN_POINT('Ctrl Pts',(12.9457680578861,-10.2392293652314,4.30878510490238));
#10624=CARTESIAN_POINT('Ctrl Pts',(12.9473704108566,-10.0014953655277,4.29592528053768));
#10625=CARTESIAN_POINT('Ctrl Pts',(12.9486079625549,-9.99993062733875,5.05407471946232));
#10626=CARTESIAN_POINT('Ctrl Pts',(12.9485059618353,-9.66120350741247,5.03577948521371));
#10627=CARTESIAN_POINT('Ctrl Pts',(13.1882325310432,-8.63670467970468,4.98043720178874));
#10628=CARTESIAN_POINT('Ctrl Pts',(14.8046014971482,-7.57922762469993,4.88804786918745));
#10629=CARTESIAN_POINT('Ctrl Pts',(16.9278971004046,-8.52299890387884,4.77690672165843));
#10630=CARTESIAN_POINT('Ctrl Pts',(17.2864719188719,-10.8187585919275,4.6657655741294));
#10631=CARTESIAN_POINT('Ctrl Pts',(15.5521007403545,-12.3650590352537,4.55462442660039));
#10632=CARTESIAN_POINT('Ctrl Pts',(13.4583451014116,-11.7867971467844,4.45072747504469));
#10633=CARTESIAN_POINT('Ctrl Pts',(12.9495010876326,-10.547171360634,4.38387757266534));
#10634=CARTESIAN_POINT('Ctrl Pts',(12.9444657818754,-9.9981973419728,4.35407471946232));
#10635=CARTESIAN_POINT('Origin',(15.,-10.,9.54592528053767));
#10636=CARTESIAN_POINT('',(12.9447204535917,-10.0018385064059,5.75407471946232));
#10637=CARTESIAN_POINT('',(12.9455806254709,-9.99812308967269,5.69592528053768));
#10638=CARTESIAN_POINT('',(12.94525,-9.99999999999991,9.54592528053767));
#10639=CARTESIAN_POINT('Ctrl Pts',(12.9455806254709,-9.99812308967269,5.69592528053768));
#10640=CARTESIAN_POINT('Ctrl Pts',(12.9440384175881,-9.82764219444215,5.68668302835179));
#10641=CARTESIAN_POINT('Ctrl Pts',(13.0414312127959,-8.97553601260769,5.64039372698956));
#10642=CARTESIAN_POINT('Ctrl Pts',(14.2260750561177,-7.69796580272048,5.55705737645098));
#10643=CARTESIAN_POINT('Ctrl Pts',(16.5143902635653,-8.10133115083163,5.44591622892198));
#10644=CARTESIAN_POINT('Ctrl Pts',(17.4164924963646,-10.2426628994423,5.33477508139295));
#10645=CARTESIAN_POINT('Ctrl Pts',(16.1066330359978,-12.161870623064,5.22363393386394));
#10646=CARTESIAN_POINT('Ctrl Pts',(13.7838054461059,-12.1021874500104,5.1124927863349));
#10647=CARTESIAN_POINT('Ctrl Pts',(12.9577392822528,-10.7472711285552,5.03658990189283));
#10648=CARTESIAN_POINT('Ctrl Pts',(12.9419578020214,-10.0338249714567,4.99773406662709));
#10649=CARTESIAN_POINT('Ctrl Pts',(12.9420873854632,-10.0006073368552,4.99592528053768));
#10650=CARTESIAN_POINT('Ctrl Pts',(12.9447204535917,-10.0018385064059,5.75407471946232));
#10651=CARTESIAN_POINT('Ctrl Pts',(12.9497105203494,-9.46110245691194,5.72472844693841));
#10652=CARTESIAN_POINT('Ctrl Pts',(13.4456630876723,-8.22963759351343,5.65833512523816));
#10653=CARTESIAN_POINT('Ctrl Pts',(15.522981873134,-7.62833192925066,5.55489475436156));
#10654=CARTESIAN_POINT('Ctrl Pts',(17.2762329089047,-9.15319233958071,5.44375360683254));
#10655=CARTESIAN_POINT('Ctrl Pts',(16.9459103296842,-11.4531869986434,5.33261245930353));
#10656=CARTESIAN_POINT('Ctrl Pts',(14.8343783693084,-12.4229917343393,5.2214713117745));
#10657=CARTESIAN_POINT('Ctrl Pts',(13.1970788393113,-11.3803396321578,5.12862539849411));
#10658=CARTESIAN_POINT('Ctrl Pts',(12.9487125088312,-10.3471111103838,5.07282653439004));
#10659=CARTESIAN_POINT('Ctrl Pts',(12.9486079625549,-9.99993062733875,5.05407471946232));
#10660=CARTESIAN_POINT('Origin',(15.,-10.,9.54592528053767));
#10661=CARTESIAN_POINT('',(12.942563023563,-9.9989300295135,6.45407471946233));
#10662=CARTESIAN_POINT('',(12.9484828432129,-10.0005308591555,6.39592528053768));
#10663=CARTESIAN_POINT('',(12.94525,-9.99999999999991,9.54592528053767));
#10664=CARTESIAN_POINT('Ctrl Pts',(12.9484828432129,-10.0005308591555,6.39592528053768));
#10665=CARTESIAN_POINT('Ctrl Pts',(12.9493515264214,-9.62486768346204,6.3756319900765));
#10666=CARTESIAN_POINT('Ctrl Pts',(13.2280330621889,-8.56220125234328,6.31829165043898));
#10667=CARTESIAN_POINT('Ctrl Pts',(14.9350675128906,-7.57222224150645,6.2239042616251));
#10668=CARTESIAN_POINT('Ctrl Pts',(17.0045371624213,-8.62881361925355,6.1127631140961));
#10669=CARTESIAN_POINT('Ctrl Pts',(17.2391327429709,-10.94053487239,6.00162196656707));
#10670=CARTESIAN_POINT('Ctrl Pts',(15.4241147373104,-12.3913276502725,5.89048081903805));
#10671=CARTESIAN_POINT('Ctrl Pts',(13.4040950937302,-11.7145752509565,5.78858192369492));
#10672=CARTESIAN_POINT('Ctrl Pts',(12.950220271332,-10.5110052949291,5.72373007752813));
#10673=CARTESIAN_POINT('Ctrl Pts',(12.9455806254709,-9.99812308967269,5.69592528053768));
#10674=CARTESIAN_POINT('Ctrl Pts',(12.942563023563,-9.9989300295135,6.45407471946233));
#10675=CARTESIAN_POINT('Ctrl Pts',(12.9421731624654,-9.93736609179818,6.45072445783946));
#10676=CARTESIAN_POINT('Ctrl Pts',(12.9726043659186,-9.19542153869923,6.41032714704025));
#10677=CARTESIAN_POINT('Ctrl Pts',(13.8720874984692,-7.84915564699463,6.3328827870647));
#10678=CARTESIAN_POINT('Ctrl Pts',(16.1953903487128,-7.88591350252874,6.22174163953568));
#10679=CARTESIAN_POINT('Ctrl Pts',(17.4244804311674,-9.85782300540329,6.11060049200668));
#10680=CARTESIAN_POINT('Ctrl Pts',(16.4342968275999,-11.959875475957,5.99945934447763));
#10681=CARTESIAN_POINT('Ctrl Pts',(14.1312146931719,-12.2679355408755,5.88831819694863));
#10682=CARTESIAN_POINT('Ctrl Pts',(13.0215194433613,-10.9668271926417,5.80652332194351));
#10683=CARTESIAN_POINT('Ctrl Pts',(12.9434110065554,-10.1437334452495,5.76177549611475));
#10684=CARTESIAN_POINT('Ctrl Pts',(12.9447204535917,-10.0018385064059,5.75407471946232));
#10685=CARTESIAN_POINT('Origin',(15.,-10.,9.54592528053767));
#10686=CARTESIAN_POINT('',(12.9479406426496,-9.99884121834684,7.15407471946232));
#10687=CARTESIAN_POINT('',(12.9436342636416,-10.0016028715607,7.09592528053768));
#10688=CARTESIAN_POINT('',(12.94525,-9.99999999999991,9.54592528053767));
#10689=CARTESIAN_POINT('Ctrl Pts',(12.9436342636416,-10.0016028715607,7.09592528053768));
#10690=CARTESIAN_POINT('Ctrl Pts',(12.9485803298624,-9.42483824360876,7.06458095180121));
#10691=CARTESIAN_POINT('Ctrl Pts',(13.5024258720897,-8.15804701499923,6.99618957388838));
#10692=CARTESIAN_POINT('Ctrl Pts',(15.6497677058271,-7.65989035373928,6.89075114679923));
#10693=CARTESIAN_POINT('Ctrl Pts',(17.3184787010345,-9.27682680041793,6.77960999927021));
#10694=CARTESIAN_POINT('Ctrl Pts',(16.8649458764968,-11.5557312969865,6.66846885174119));
#10695=CARTESIAN_POINT('Ctrl Pts',(14.7043153699076,-12.4105788623587,6.55732770421217));
#10696=CARTESIAN_POINT('Ctrl Pts',(13.1594334243237,-11.3056861225605,6.46647984714433));
#10697=CARTESIAN_POINT('Ctrl Pts',(12.9477656747032,-10.3106713075848,6.41267903925284));
#10698=CARTESIAN_POINT('Ctrl Pts',(12.9484828432129,-10.0005308591555,6.39592528053768));
#10699=CARTESIAN_POINT('Ctrl Pts',(12.9479406426496,-9.99884121834684,7.15407471946232));
#10700=CARTESIAN_POINT('Ctrl Pts',(12.9465639668134,-9.73242150920767,7.13967341956416));
#10701=CARTESIAN_POINT('Ctrl Pts',(13.1185706050062,-8.78234603046162,7.08822507048967));
#10702=CARTESIAN_POINT('Ctrl Pts',(14.5523165742456,-7.61298740370139,6.99972967223882));
#10703=CARTESIAN_POINT('Ctrl Pts',(16.7627158202625,-8.32932372056038,6.88858852470981));
#10704=CARTESIAN_POINT('Ctrl Pts',(17.3596103902574,-10.5749548405481,6.77744737718078));
#10705=CARTESIAN_POINT('Ctrl Pts',(15.7966027972857,-12.2942827529436,6.66630622965177));
#10706=CARTESIAN_POINT('Ctrl Pts',(13.5735166885531,-11.9249990288555,6.55851534374561));
#10707=CARTESIAN_POINT('Ctrl Pts',(12.9464842297429,-10.6181374716992,6.4877715070158));
#10708=CARTESIAN_POINT('Ctrl Pts',(12.942563023563,-9.9989300295135,6.45407471946233));
#10709=CARTESIAN_POINT('Origin',(15.,-10.,9.54592528053767));
#10710=CARTESIAN_POINT('',(12.9473113312417,-10.0024712008536,7.85407471946232));
#10711=CARTESIAN_POINT('',(12.9434529369556,-9.99851181185547,7.79592528053768));
#10712=CARTESIAN_POINT('',(12.94525,-9.99999999999991,9.54592528053767));
#10713=CARTESIAN_POINT('',(14.4698297828114,-11.9851743256717,8.));
#10714=CARTESIAN_POINT('Ctrl Pts',(14.4698297828114,-11.9851743256717,8.));
#10715=CARTESIAN_POINT('Ctrl Pts',(13.8096927451188,-11.8088749487748,7.96295295082366));
#10716=CARTESIAN_POINT('Ctrl Pts',(13.0749951173004,-11.1129906421843,7.91431119064443));
#10717=CARTESIAN_POINT('Ctrl Pts',(12.9456876260347,-10.2167165909839,7.86566943046521));
#10718=CARTESIAN_POINT('Ctrl Pts',(12.9473113312417,-10.0024712008536,7.85407471946232));
#10719=CARTESIAN_POINT('',(15.5312697408697,-11.9887498021333,8.));
#10720=CARTESIAN_POINT('Origin',(15.,-10.,8.));
#10721=CARTESIAN_POINT('Ctrl Pts',(15.5312701240486,-11.9887510481705,8.));
#10722=CARTESIAN_POINT('Ctrl Pts',(14.8865854870743,-12.1601151282119,7.96367382485347));
#10723=CARTESIAN_POINT('Ctrl Pts',(13.5069338574846,-11.8405010530347,7.89564891836603));
#10724=CARTESIAN_POINT('Ctrl Pts',(12.948322230655,-10.581516770577,7.82762401187859));
#10725=CARTESIAN_POINT('Ctrl Pts',(12.9434529369556,-9.99851181185547,7.79592528053768));
#10726=CARTESIAN_POINT('Origin',(-15.,10.,9.54592528053767));
#10727=CARTESIAN_POINT('',(-17.051781505051,10.0008196635194,0.154074719462318));
#10728=CARTESIAN_POINT('',(-17.0565587168069,9.99843575839028,0.0959252805376745));
#10729=CARTESIAN_POINT('',(-17.05475,10.0000000000001,9.54592528053767));
#10730=CARTESIAN_POINT('',(-16.3390017195986,11.5585480285869,0.));
#10731=CARTESIAN_POINT('Ctrl Pts',(-17.0565587168069,9.99843575839027,0.0959252805376745));
#10732=CARTESIAN_POINT('Ctrl Pts',(-17.0518110208044,10.5850503744189,0.0639501870251164));
#10733=CARTESIAN_POINT('Ctrl Pts',(-16.7863171109466,11.1742441334025,0.0319750935125583));
#10734=CARTESIAN_POINT('Ctrl Pts',(-16.3390017195986,11.5585480285869,0.));
#10735=CARTESIAN_POINT('',(-15.3842290273038,12.0223109749866,-1.12886049415522E-15));
#10736=CARTESIAN_POINT('Origin',(-15.,10.,0.));
#10737=CARTESIAN_POINT('Ctrl Pts',(-17.051781505051,10.0008196635194,0.154074719462318));
#10738=CARTESIAN_POINT('Ctrl Pts',(-17.0529878932198,10.2789132148305,0.139042654788076));
#10739=CARTESIAN_POINT('Ctrl Pts',(-16.8731947834857,11.2276339555148,0.0876844149673036));
#10740=CARTESIAN_POINT('Ctrl Pts',(-16.0394222823928,11.8969878319988,0.0363261751465303));
#10741=CARTESIAN_POINT('Ctrl Pts',(-15.384229221931,12.022312258029,-5.35595873207839E-16));
#10742=CARTESIAN_POINT('Origin',(-15.,10.,9.54592528053767));
#10743=CARTESIAN_POINT('',(-17.0535052107051,9.99822649184017,0.854074719462319));
#10744=CARTESIAN_POINT('',(-17.0562188773561,10.0016641224949,0.795925280537675));
#10745=CARTESIAN_POINT('',(-17.05475,10.0000000000001,9.54592528053767));
#10746=CARTESIAN_POINT('Ctrl Pts',(-17.0562188773561,10.0016641224949,0.795925280537675));
#10747=CARTESIAN_POINT('Ctrl Pts',(-17.0571796395141,10.1117045841504,0.789946197926163));
#10748=CARTESIAN_POINT('Ctrl Pts',(-16.9990975224492,10.9025459743661,0.746920066138311));
#10749=CARTESIAN_POINT('Ctrl Pts',(-15.9729747466193,12.225122550715,0.66684688517412));
#10750=CARTESIAN_POINT('Ctrl Pts',(-13.6580451964401,12.0244599984212,0.555705737645099));
#10751=CARTESIAN_POINT('Ctrl Pts',(-12.5715926312396,9.9699163594395,0.444564590116078));
#10752=CARTESIAN_POINT('Ctrl Pts',(-13.7078058101514,7.94440559808363,0.333423442587059));
#10753=CARTESIAN_POINT('Ctrl Pts',(-16.0272308405357,7.79758227864481,0.222282295058039));
#10754=CARTESIAN_POINT('Ctrl Pts',(-17.0090843242089,9.13320995690963,0.143116241041577));
#10755=CARTESIAN_POINT('Ctrl Pts',(-17.0573118061957,9.90538573109153,0.100997236201456));
#10756=CARTESIAN_POINT('Ctrl Pts',(-17.0565587168069,9.99843575839027,0.0959252805376745));
#10757=CARTESIAN_POINT('Ctrl Pts',(-17.0535052107051,9.99822649184017,0.854074719462319));
#10758=CARTESIAN_POINT('Ctrl Pts',(-17.0495358029268,10.4798921752139,0.827991616512783));
#10759=CARTESIAN_POINT('Ctrl Pts',(-16.6400832266998,11.6517646154016,0.764861464386908));
#10760=CARTESIAN_POINT('Ctrl Pts',(-14.6871808849242,12.408440519574,0.664684263084692));
#10761=CARTESIAN_POINT('Ctrl Pts',(-12.8068360443054,11.0432447977232,0.553543115555672));
#10762=CARTESIAN_POINT('Ctrl Pts',(-12.9341204463425,8.72328850320409,0.442401968026654));
#10763=CARTESIAN_POINT('Ctrl Pts',(-14.9522477729176,7.57162591585277,0.331260820497632));
#10764=CARTESIAN_POINT('Ctrl Pts',(-16.7355222628146,8.49852169035672,0.235151737642854));
#10765=CARTESIAN_POINT('Ctrl Pts',(-17.0500147073812,9.59354193055857,0.176089703964416));
#10766=CARTESIAN_POINT('Ctrl Pts',(-17.051781505051,10.0008196635194,0.154074719462318));
#10767=CARTESIAN_POINT('Origin',(-15.,10.,9.54592528053767));
#10768=CARTESIAN_POINT('',(-17.0581308917344,10.0000299187367,1.55407471946232));
#10769=CARTESIAN_POINT('',(-17.0514805469147,10.0004498953059,1.49592528053768));
#10770=CARTESIAN_POINT('',(-17.05475,10.0000000000001,9.54592528053767));
#10771=CARTESIAN_POINT('Ctrl Pts',(-17.0514805469147,10.0004498953059,1.49592528053768));
#10772=CARTESIAN_POINT('Ctrl Pts',(-17.0520974357427,10.3157203081079,1.47889515965087));
#10773=CARTESIAN_POINT('Ctrl Pts',(-16.8355232105105,11.3160213722625,1.42481798958772));
#10774=CARTESIAN_POINT('Ctrl Pts',(-15.277737680073,12.4127105190431,1.33369377034824));
#10775=CARTESIAN_POINT('Ctrl Pts',(-13.1235279142844,11.5418130937198,1.22255262281922));
#10776=CARTESIAN_POINT('Ctrl Pts',(-12.6869684838201,9.25958637970326,1.1114114752902));
#10777=CARTESIAN_POINT('Ctrl Pts',(-14.3676628265377,7.65513319733112,1.00027032776118));
#10778=CARTESIAN_POINT('Ctrl Pts',(-16.5056252839035,8.16787157989892,0.895108262843672));
#10779=CARTESIAN_POINT('Ctrl Pts',(-17.0512266522036,9.42988185995992,0.826993247102503));
#10780=CARTESIAN_POINT('Ctrl Pts',(-17.0562188773561,10.0016641224949,0.795925280537675));
#10781=CARTESIAN_POINT('Ctrl Pts',(-17.0581308917344,10.0000299187367,1.55407471946232));
#10782=CARTESIAN_POINT('Ctrl Pts',(-17.0581312349042,10.0016288743118,1.55398762741383));
#10783=CARTESIAN_POINT('Ctrl Pts',(-17.0574054212678,10.6833881760579,1.516853486189));
#10784=CARTESIAN_POINT('Ctrl Pts',(-16.3123135322607,12.0435636244015,1.44267229578783));
#10785=CARTESIAN_POINT('Ctrl Pts',(-13.9947484023904,12.2108350155113,1.33153114825881));
#10786=CARTESIAN_POINT('Ctrl Pts',(-12.5973499293358,10.3543936440402,1.22039000072979));
#10787=CARTESIAN_POINT('Ctrl Pts',(-13.3992441080921,8.17355782375309,1.10924885320077));
#10788=CARTESIAN_POINT('Ctrl Pts',(-15.6664035170272,7.66456821418318,0.998107705671752));
#10789=CARTESIAN_POINT('Ctrl Pts',(-16.9346588395231,8.91110294463132,0.913049661092267));
#10790=CARTESIAN_POINT('Ctrl Pts',(-17.055173738162,9.79575991177017,0.865038665689123));
#10791=CARTESIAN_POINT('Ctrl Pts',(-17.0535052107051,9.99822649184017,0.854074719462319));
#10792=CARTESIAN_POINT('Origin',(-15.,10.,9.54592528053767));
#10793=CARTESIAN_POINT('',(-17.0534183096233,10.0017541282783,2.25407471946232));
#10794=CARTESIAN_POINT('',(-17.054572101898,9.99812063734445,2.19592528053768));
#10795=CARTESIAN_POINT('',(-17.05475,10.0000000000001,9.54592528053767));
#10796=CARTESIAN_POINT('Ctrl Pts',(-17.054572101898,9.99812063734445,2.19592528053768));
#10797=CARTESIAN_POINT('Ctrl Pts',(-17.0498495609752,10.5160021919663,2.16784412137558));
#10798=CARTESIAN_POINT('Ctrl Pts',(-16.5885931165834,11.7246094338528,2.10271591303714));
#10799=CARTESIAN_POINT('Ctrl Pts',(-14.5581012780927,12.3881050358458,2.00054065552236));
#10800=CARTESIAN_POINT('Ctrl Pts',(-12.7539301588106,10.9238456569314,1.88939950799334));
#10801=CARTESIAN_POINT('Ctrl Pts',(-13.0057226092633,8.61393421415536,1.77825836046432));
#10802=CARTESIAN_POINT('Ctrl Pts',(-15.0829976655305,7.57277312445451,1.6671172129353));
#10803=CARTESIAN_POINT('Ctrl Pts',(-16.7776411801768,8.57249168811958,1.57300618629308));
#10804=CARTESIAN_POINT('Ctrl Pts',(-17.0507554657768,9.6298861578658,1.51594220882721));
#10805=CARTESIAN_POINT('Ctrl Pts',(-17.0514805469147,10.0004498953059,1.49592528053768));
#10806=CARTESIAN_POINT('Ctrl Pts',(-17.0534183096233,10.0017541282783,2.25407471946232));
#10807=CARTESIAN_POINT('Ctrl Pts',(-17.0550897179391,10.2074604490073,2.24293658913854));
#10808=CARTESIAN_POINT('Ctrl Pts',(-16.9321369327745,11.0954235474083,2.19475140963841));
#10809=CARTESIAN_POINT('Ctrl Pts',(-15.655443965717,12.3385281044116,2.10951918096195));
#10810=CARTESIAN_POINT('Ctrl Pts',(-13.3906939975623,11.8189158098855,1.99837803343293));
#10811=CARTESIAN_POINT('Ctrl Pts',(-12.5990391016035,9.63433986139397,1.88723688590391));
#10812=CARTESIAN_POINT('Ctrl Pts',(-14.0051289214666,7.7844748128269,1.77609573837489));
#10813=CARTESIAN_POINT('Ctrl Pts',(-16.3200688809162,7.96247420798835,1.66504168289436));
#10814=CARTESIAN_POINT('Ctrl Pts',(-17.0579852579768,9.3214682069898,1.59103467659017));
#10815=CARTESIAN_POINT('Ctrl Pts',(-17.0581308917344,10.0000299187367,1.55407471946232));
#10816=CARTESIAN_POINT('Origin',(-15.,10.,9.54592528053767));
#10817=CARTESIAN_POINT('',(-17.0519255652782,9.99894822627429,2.95407471946232));
#10818=CARTESIAN_POINT('',(-17.0578444035932,10.0006952919057,2.89592528053767));
#10819=CARTESIAN_POINT('',(-17.05475,10.0000000000001,9.54592528053767));
#10820=CARTESIAN_POINT('Ctrl Pts',(-17.0578444035932,10.0006952919057,2.89592528053767));
#10821=CARTESIAN_POINT('Ctrl Pts',(-17.0580127536815,10.0389915801255,2.89384013227662));
#10822=CARTESIAN_POINT('Ctrl Pts',(-17.0396873009863,10.7575377341649,2.85470793483923));
#10823=CARTESIAN_POINT('Ctrl Pts',(-16.2005167352846,12.1111797432876,2.7785286882255));
#10824=CARTESIAN_POINT('Ctrl Pts',(-13.8773094989449,12.1535752538516,2.66738754069648));
#10825=CARTESIAN_POINT('Ctrl Pts',(-12.5817687604279,10.2246731230589,2.55624639316746));
#10826=CARTESIAN_POINT('Ctrl Pts',(-13.4997812925854,8.09011409287,2.44510524563844));
#10827=CARTESIAN_POINT('Ctrl Pts',(-15.7910347157817,7.70378912322181,2.33396409810942));
#10828=CARTESIAN_POINT('Ctrl Pts',(-16.9622413410058,8.98587389146773,2.2509041097425));
#10829=CARTESIAN_POINT('Ctrl Pts',(-17.0560799378907,9.83276887845376,2.20489117055192));
#10830=CARTESIAN_POINT('Ctrl Pts',(-17.054572101898,9.99812063734445,2.19592528053768));
#10831=CARTESIAN_POINT('Ctrl Pts',(-17.0519255652782,9.99894822627429,2.95407471946232));
#10832=CARTESIAN_POINT('Ctrl Pts',(-17.0500217756369,10.4095028825701,2.93188555086324));
#10833=CARTESIAN_POINT('Ctrl Pts',(-16.7315452143008,11.5082393895864,2.87264933308783));
#10834=CARTESIAN_POINT('Ctrl Pts',(-14.9409585995702,12.4279280521305,2.77636606613606));
#10835=CARTESIAN_POINT('Ctrl Pts',(-12.9281031098292,11.2671084366828,2.66522491860705));
#10836=CARTESIAN_POINT('Ctrl Pts',(-12.8117801189011,8.94642785381579,2.55408377107803));
#10837=CARTESIAN_POINT('Ctrl Pts',(-14.6984670947123,7.59014556097653,2.44294262354901));
#10838=CARTESIAN_POINT('Ctrl Pts',(-16.6444282224071,8.35460484167498,2.34293960634377));
#10839=CARTESIAN_POINT('Ctrl Pts',(-17.0495303696222,9.52325116446895,2.27998363831488));
#10840=CARTESIAN_POINT('Ctrl Pts',(-17.0534183096233,10.0017541282783,2.25407471946232));
#10841=CARTESIAN_POINT('Origin',(-15.,10.,9.54592528053767));
#10842=CARTESIAN_POINT('',(-17.0572564748192,9.99880853407964,3.65407471946232));
#10843=CARTESIAN_POINT('',(-17.0525171838174,10.0014423098,3.59592528053768));
#10844=CARTESIAN_POINT('',(-17.05475,10.0000000000001,9.54592528053767));
#10845=CARTESIAN_POINT('Ctrl Pts',(-17.0525171838174,10.0014423098,3.59592528053768));
#10846=CARTESIAN_POINT('Ctrl Pts',(-17.054090358096,10.2443186665424,3.58278909400133));
#10847=CARTESIAN_POINT('Ctrl Pts',(-16.9018844793529,11.1702542247926,3.53260585828864));
#10848=CARTESIAN_POINT('Ctrl Pts',(-15.5287351174808,12.3703922701155,3.44537557339962));
#10849=CARTESIAN_POINT('Ctrl Pts',(-13.2952058971985,11.7297391149084,3.33423442587059));
#10850=CARTESIAN_POINT('Ctrl Pts',(-12.6221777981957,9.50575116060393,3.22309327834158));
#10851=CARTESIAN_POINT('Ctrl Pts',(-14.125714133608,7.73417905325592,3.11195213081255));
#10852=CARTESIAN_POINT('Ctrl Pts',(-16.3863145560916,8.03097512543151,3.00289613154459));
#10853=CARTESIAN_POINT('Ctrl Pts',(-17.0550216598983,9.35857738634755,2.93088718145296));
#10854=CARTESIAN_POINT('Ctrl Pts',(-17.0578444035932,10.0006952919057,2.89592528053767));
#10855=CARTESIAN_POINT('Ctrl Pts',(-17.0572564748192,9.99880853407964,3.65407471946232));
#10856=CARTESIAN_POINT('Ctrl Pts',(-17.0530395431727,10.6097671369969,3.62083451258795));
#10857=CARTESIAN_POINT('Ctrl Pts',(-16.440646393087,11.9089948838,3.55054725653724));
#10858=CARTESIAN_POINT('Ctrl Pts',(-14.2316631634768,12.3039051671823,3.44321295131019));
#10859=CARTESIAN_POINT('Ctrl Pts',(-12.647638749453,10.6039180910149,3.33207180378117));
#10860=CARTESIAN_POINT('Ctrl Pts',(-13.2168728216632,8.35112827071217,3.22093065625215));
#10861=CARTESIAN_POINT('Ctrl Pts',(-15.4183110155551,7.60765044194128,3.10978950872313));
#10862=CARTESIAN_POINT('Ctrl Pts',(-16.8737764074476,8.76526627680962,3.02083752979319));
#10863=CARTESIAN_POINT('Ctrl Pts',(-17.0532003439618,9.72404058264425,2.96893260003958));
#10864=CARTESIAN_POINT('Ctrl Pts',(-17.0519255652782,9.99894822627429,2.95407471946232));
#10865=CARTESIAN_POINT('Origin',(-15.,10.,9.54592528053767));
#10866=CARTESIAN_POINT('',(-17.0555344003932,10.001802658187,4.35407471946232));
#10867=CARTESIAN_POINT('',(-17.0526294274916,9.99850463459006,4.29592528053768));
#10868=CARTESIAN_POINT('',(-17.05475,10.0000000000001,9.54592528053767));
#10869=CARTESIAN_POINT('Ctrl Pts',(-17.0526294274916,9.99850463459006,4.29592528053768));
#10870=CARTESIAN_POINT('Ctrl Pts',(-17.0496156640549,10.4456433419542,4.27173805572604));
#10871=CARTESIAN_POINT('Ctrl Pts',(-16.6860606566458,11.5821157981759,4.21050378173806));
#10872=CARTESIAN_POINT('Ctrl Pts',(-14.8104759510498,12.4212395531045,4.11222245857373));
#10873=CARTESIAN_POINT('Ctrl Pts',(-12.8629592808463,11.1538532416754,4.00108131104471));
#10874=CARTESIAN_POINT('Ctrl Pts',(-12.8716051953172,8.83027529134189,3.8899401635157));
#10875=CARTESIAN_POINT('Ctrl Pts',(-14.8284995661796,7.57741709329663,3.77879901598667));
#10876=CARTESIAN_POINT('Ctrl Pts',(-16.6925314043128,8.42807657117643,3.68079405499401));
#10877=CARTESIAN_POINT('Ctrl Pts',(-17.0496536469772,9.55935181508152,3.61983614317767));
#10878=CARTESIAN_POINT('Ctrl Pts',(-17.0525171838174,10.0014423098,3.59592528053768));
#10879=CARTESIAN_POINT('Ctrl Pts',(-17.0555344003932,10.001802658187,4.35407471946232));
#10880=CARTESIAN_POINT('Ctrl Pts',(-17.0567583350506,10.1352420876602,4.346830523489));
#10881=CARTESIAN_POINT('Ctrl Pts',(-16.9841132410514,10.9497682650209,4.30253927833933));
#10882=CARTESIAN_POINT('Ctrl Pts',(-15.8966027914863,12.2570830618385,4.22120098401332));
#10883=CARTESIAN_POINT('Ctrl Pts',(-13.5899070517775,11.9773614720396,4.11005983648431));
#10884=CARTESIAN_POINT('Ctrl Pts',(-12.5739546477039,9.8876413673274,3.99891868895528));
#10885=CARTESIAN_POINT('Ctrl Pts',(-13.7787082434502,7.90076991277298,3.88777754142627));
#10886=CARTESIAN_POINT('Ctrl Pts',(-16.1013840283822,7.83545068530234,3.77663639389724));
#10887=CARTESIAN_POINT('Ctrl Pts',(-17.0227507221578,9.1784280346853,3.6987354532426));
#10888=CARTESIAN_POINT('Ctrl Pts',(-17.0577394198814,9.92883836021378,3.65788156176429));
#10889=CARTESIAN_POINT('Ctrl Pts',(-17.0572564748192,9.99880853407964,3.65407471946232));
#10890=CARTESIAN_POINT('Origin',(-15.,10.,9.54592528053767));
#10891=CARTESIAN_POINT('',(-17.0513922193463,10.0000693726672,5.05407471946232));
#10892=CARTESIAN_POINT('',(-17.0579124524689,9.99939266319272,4.99592528053768));
#10893=CARTESIAN_POINT('',(-17.05475,10.0000000000001,9.54592528053767));
#10894=CARTESIAN_POINT('Ctrl Pts',(-17.0579124524689,9.99939266319272,4.99592528053768));
#10895=CARTESIAN_POINT('Ctrl Pts',(-17.0553879444141,10.6465292493746,4.96068701745074));
#10896=CARTESIAN_POINT('Ctrl Pts',(-16.3773571856509,11.9785775515288,4.88840170518747));
#10897=CARTESIAN_POINT('Ctrl Pts',(-14.1088765692626,12.2592519491796,4.77906934374786));
#10898=CARTESIAN_POINT('Ctrl Pts',(-12.6185655430924,10.4765398893022,4.66792819621883));
#10899=CARTESIAN_POINT('Ctrl Pts',(-13.3081254668317,8.25762205516231,4.55678704868981));
#10900=CARTESIAN_POINT('Ctrl Pts',(-15.5463604486011,7.63360810539413,4.44564590116079));
#10901=CARTESIAN_POINT('Ctrl Pts',(-16.9062186237658,8.84009707796262,4.35869197844341));
#10902=CARTESIAN_POINT('Ctrl Pts',(-17.0542317803359,9.76077065360876,4.30878510490238));
#10903=CARTESIAN_POINT('Ctrl Pts',(-17.0526294274916,9.99850463459006,4.29592528053768));
#10904=CARTESIAN_POINT('Ctrl Pts',(-17.0513922193463,10.0000693726672,5.05407471946232));
#10905=CARTESIAN_POINT('Ctrl Pts',(-17.051494220075,10.3387965226292,5.0357794852137));
#10906=CARTESIAN_POINT('Ctrl Pts',(-16.8117676296103,11.3632954411821,4.98043720178875));
#10907=CARTESIAN_POINT('Ctrl Pts',(-15.195398520178,12.4207725899548,4.88804786918745));
#10908=CARTESIAN_POINT('Ctrl Pts',(-13.0721027286448,11.4770012270902,4.77690672165843));
#10909=CARTESIAN_POINT('Ctrl Pts',(-12.7135278783817,9.18124133547139,4.66576557412941));
#10910=CARTESIAN_POINT('Ctrl Pts',(-14.4478992106895,7.63494075503149,4.55462442660039));
#10911=CARTESIAN_POINT('Ctrl Pts',(-16.5416550352902,8.21320269477644,4.45072747504469));
#10912=CARTESIAN_POINT('Ctrl Pts',(-17.0504990941895,9.45282859084715,4.38387757266534));
#10913=CARTESIAN_POINT('Ctrl Pts',(-17.0555344003932,10.001802658187,4.35407471946232));
#10914=CARTESIAN_POINT('Origin',(-15.,10.,9.54592528053767));
#10915=CARTESIAN_POINT('',(-17.0552797286464,9.99816149341417,5.75407471946232));
#10916=CARTESIAN_POINT('',(-17.0544192127363,10.0018769101795,5.69592528053768));
#10917=CARTESIAN_POINT('',(-17.05475,10.0000000000001,9.54592528053767));
#10918=CARTESIAN_POINT('Ctrl Pts',(-17.0544192127363,10.0018769101795,5.69592528053768));
#10919=CARTESIAN_POINT('Ctrl Pts',(-17.0559614204976,10.172357791985,5.68668302835179));
#10920=CARTESIAN_POINT('Ctrl Pts',(-16.9585686329592,11.0244639067171,5.64039372698956));
#10921=CARTESIAN_POINT('Ctrl Pts',(-15.7739248829336,12.3020340159819,5.557057376451));
#10922=CARTESIAN_POINT('Ctrl Pts',(-13.485609855698,11.8986686996438,5.44591622892196));
#10923=CARTESIAN_POINT('Ctrl Pts',(-12.5835076939429,9.75733711966703,5.33477508139296));
#10924=CARTESIAN_POINT('Ctrl Pts',(-13.8933670511534,7.83812954719161,5.22363393386392));
#10925=CARTESIAN_POINT('Ctrl Pts',(-16.2161944581144,7.89781271554394,5.11249278633492));
#10926=CARTESIAN_POINT('Ctrl Pts',(-17.0422605569119,9.25272893029508,5.03658990189283));
#10927=CARTESIAN_POINT('Ctrl Pts',(-17.0580420359005,9.96617503120721,4.99773406662709));
#10928=CARTESIAN_POINT('Ctrl Pts',(-17.0579124524689,9.99939266319272,4.99592528053768));
#10929=CARTESIAN_POINT('Ctrl Pts',(-17.0552797286464,9.99816149341417,5.75407471946232));
#10930=CARTESIAN_POINT('Ctrl Pts',(-17.050289661447,10.5388975908579,5.72472844693841));
#10931=CARTESIAN_POINT('Ctrl Pts',(-16.5543370501663,11.7703625634938,5.65833512523816));
#10932=CARTESIAN_POINT('Ctrl Pts',(-14.4770180804847,12.3716682810349,5.55489475436156));
#10933=CARTESIAN_POINT('Ctrl Pts',(-12.7237668892609,10.8468077355158,5.44375360683255));
#10934=CARTESIAN_POINT('Ctrl Pts',(-13.0540894977656,8.54681287249504,5.33261245930352));
#10935=CARTESIAN_POINT('Ctrl Pts',(-15.1656216453787,7.57700805081118,5.22147131177451));
#10936=CARTESIAN_POINT('Ctrl Pts',(-16.8029213205572,8.61966024544381,5.1286253984941));
#10937=CARTESIAN_POINT('Ctrl Pts',(-17.0512876730606,9.65288885883676,5.07282653439004));
#10938=CARTESIAN_POINT('Ctrl Pts',(-17.0513922193463,10.0000693726672,5.05407471946232));
#10939=CARTESIAN_POINT('Origin',(-15.,10.,9.54592528053767));
#10940=CARTESIAN_POINT('',(-17.0574371586977,10.0010699701727,6.45407471946232));
#10941=CARTESIAN_POINT('',(-17.0515169952491,9.99946914075972,6.39592528053768));
#10942=CARTESIAN_POINT('',(-17.05475,10.0000000000001,9.54592528053767));
#10943=CARTESIAN_POINT('Ctrl Pts',(-17.0515169952491,9.99946914075972,6.39592528053768));
#10944=CARTESIAN_POINT('Ctrl Pts',(-17.050648312096,10.3751322869369,6.3756319900765));
#10945=CARTESIAN_POINT('Ctrl Pts',(-16.7719667982161,11.4377986346686,6.31829165043897));
#10946=CARTESIAN_POINT('Ctrl Pts',(-15.0649324820269,12.4277775671245,6.22390426162511));
#10947=CARTESIAN_POINT('Ctrl Pts',(-12.9954629954269,11.3711862728547,6.11276311409609));
#10948=CARTESIAN_POINT('Ctrl Pts',(-12.7608674333771,9.05946520162959,6.00162196656707));
#10949=CARTESIAN_POINT('Ctrl Pts',(-14.5758852960858,7.60867253808055,5.89048081903805));
#10950=CARTESIAN_POINT('Ctrl Pts',(-16.5959047805884,8.285424884061,5.78858192369492));
#10951=CARTESIAN_POINT('Ctrl Pts',(-17.0497795672411,9.48899474531162,5.72373007752813));
#10952=CARTESIAN_POINT('Ctrl Pts',(-17.0544192127363,10.0018769101795,5.69592528053768));
#10953=CARTESIAN_POINT('Ctrl Pts',(-17.0574371586977,10.0010699701727,6.45407471946233));
#10954=CARTESIAN_POINT('Ctrl Pts',(-17.0578270198062,10.0626339132856,6.45072445783946));
#10955=CARTESIAN_POINT('Ctrl Pts',(-17.027395813414,10.8045785315454,6.41032714704025));
#10956=CARTESIAN_POINT('Ctrl Pts',(-16.1279126020198,12.1508445448559,6.33288278706471));
#10957=CARTESIAN_POINT('Ctrl Pts',(-13.8046095450231,12.114086684316,6.22174163953567));
#10958=CARTESIAN_POINT('Ctrl Pts',(-12.5755193539972,10.1421770075384,6.11060049200667));
#10959=CARTESIAN_POINT('Ctrl Pts',(-13.5657030451356,8.04012435007543,5.99945934447765));
#10960=CARTESIAN_POINT('Ctrl Pts',(-15.8687853839106,7.73206425811983,5.88831819694862));
#10961=CARTESIAN_POINT('Ctrl Pts',(-16.9784807320684,9.03317272161465,5.80652332194352));
#10962=CARTESIAN_POINT('Ctrl Pts',(-17.0565891757986,9.85626654198804,5.76177549611475));
#10963=CARTESIAN_POINT('Ctrl Pts',(-17.0552797286464,9.99816149341417,5.75407471946232));
#10964=CARTESIAN_POINT('Origin',(-15.,10.,9.54592528053767));
#10965=CARTESIAN_POINT('',(-17.0520595406494,10.0011587933795,7.15407471946233));
#10966=CARTESIAN_POINT('',(-17.0563655762952,9.99839712210779,7.09592528053768));
#10967=CARTESIAN_POINT('',(-17.05475,10.0000000000001,9.54592528053767));
#10968=CARTESIAN_POINT('Ctrl Pts',(-17.0563655762952,9.99839712210779,7.09592528053768));
#10969=CARTESIAN_POINT('Ctrl Pts',(-17.0514195106288,10.575161704561,7.0645809518012));
#10970=CARTESIAN_POINT('Ctrl Pts',(-16.4975740071439,11.8419528502525,6.99618957388838));
#10971=CARTESIAN_POINT('Ctrl Pts',(-14.3502323469365,12.3401094557021,6.89075114679924));
#10972=CARTESIAN_POINT('Ctrl Pts',(-12.6815214807272,10.7231731461125,6.77960999927021));
#10973=CARTESIAN_POINT('Ctrl Pts',(-13.1350542708035,8.44426882360712,6.66846885174119));
#10974=CARTESIAN_POINT('Ctrl Pts',(-15.2956846065833,7.58942132854296,6.55732770421217));
#10975=CARTESIAN_POINT('Ctrl Pts',(-16.8405664307791,8.69431397998541,6.46647984714433));
#10976=CARTESIAN_POINT('Ctrl Pts',(-17.0522341637131,9.68932871669844,6.41267903925284));
#10977=CARTESIAN_POINT('Ctrl Pts',(-17.0515169952491,9.99946914075972,6.39592528053768));
#10978=CARTESIAN_POINT('Ctrl Pts',(-17.0520595406494,10.0011587933795,7.15407471946232));
#10979=CARTESIAN_POINT('Ctrl Pts',(-17.0534362134906,10.2675785134614,7.13967341956416));
#10980=CARTESIAN_POINT('Ctrl Pts',(-16.8814295491932,11.2176540291726,7.08822507048967));
#10981=CARTESIAN_POINT('Ctrl Pts',(-15.447683477411,12.3870128478829,6.99972967223881));
#10982=CARTESIAN_POINT('Ctrl Pts',(-13.2372840161297,11.670676405265,6.88858852470981));
#10983=CARTESIAN_POINT('Ctrl Pts',(-12.6403894048645,9.42504512087116,6.77744737718078));
#10984=CARTESIAN_POINT('Ctrl Pts',(-14.2033971295295,7.70571703676082,6.66630622965177));
#10985=CARTESIAN_POINT('Ctrl Pts',(-16.4264834392857,8.07500080390432,6.55851534374561));
#10986=CARTESIAN_POINT('Ctrl Pts',(-17.0535159524081,9.38186247369755,6.4877715070158));
#10987=CARTESIAN_POINT('Ctrl Pts',(-17.0574371586977,10.0010699701727,6.45407471946233));
#10988=CARTESIAN_POINT('Origin',(-15.,10.,9.54592528053767));
#10989=CARTESIAN_POINT('',(-17.052688542414,9.99752997529134,7.85407471946233));
#10990=CARTESIAN_POINT('',(-17.056546936061,10.0014880949897,7.79592528053768));
#10991=CARTESIAN_POINT('',(-17.05475,10.0000000000001,9.54592528053767));
#10992=CARTESIAN_POINT('',(-15.5301702171886,8.01482567432828,8.));
#10993=CARTESIAN_POINT('Ctrl Pts',(-15.5301702171886,8.01482567432828,8.));
#10994=CARTESIAN_POINT('Ctrl Pts',(-16.1903072548812,8.1911250512252,7.96295295082366));
#10995=CARTESIAN_POINT('Ctrl Pts',(-16.9250045409916,8.88701144695482,7.91431119064444));
#10996=CARTESIAN_POINT('Ctrl Pts',(-17.0543121964904,9.78328481586603,7.86566943046521));
#10997=CARTESIAN_POINT('Ctrl Pts',(-17.052688542414,9.99752997529134,7.85407471946233));
#10998=CARTESIAN_POINT('',(-14.4687306105943,8.01125000725434,8.));
#10999=CARTESIAN_POINT('Origin',(-15.,10.,8.));
#11000=CARTESIAN_POINT('Ctrl Pts',(-14.4687302296836,8.0112487681312,8.));
#11001=CARTESIAN_POINT('Ctrl Pts',(-15.1134150435372,7.83988452957895,7.96367382485347));
#11002=CARTESIAN_POINT('Ctrl Pts',(-16.4930655292016,8.15949974734112,7.89564891836604));
#11003=CARTESIAN_POINT('Ctrl Pts',(-17.0516775383829,9.41848331501726,7.82762401187859));
#11004=CARTESIAN_POINT('Ctrl Pts',(-17.056546936061,10.0014880949897,7.79592528053768));
#11005=CARTESIAN_POINT('Origin',(15.,10.,9.54592528053767));
#11006=CARTESIAN_POINT('',(12.9482186935975,10.0008196174515,0.15407471946232));
#11007=CARTESIAN_POINT('',(12.943442368457,9.99843416552646,0.0959252805376746));
#11008=CARTESIAN_POINT('',(12.94525,10.0000000000001,9.54592528053767));
#11009=CARTESIAN_POINT('',(13.6609982804014,11.5585480285869,0.));
#11010=CARTESIAN_POINT('Ctrl Pts',(12.943442368457,9.99843416552646,0.0959252805376745));
#11011=CARTESIAN_POINT('Ctrl Pts',(12.9481898548418,10.5850491239192,0.0639501870251164));
#11012=CARTESIAN_POINT('Ctrl Pts',(13.2136828890534,11.1742441334025,0.0319750935125583));
#11013=CARTESIAN_POINT('Ctrl Pts',(13.6609982804014,11.5585480285869,0.));
#11014=CARTESIAN_POINT('',(14.6157707560785,12.0223109855879,-5.36454528360574E-16));
#11015=CARTESIAN_POINT('Origin',(15.,10.,0.));
#11016=CARTESIAN_POINT('Ctrl Pts',(12.9482186935975,10.0008196174515,0.15407471946232));
#11017=CARTESIAN_POINT('Ctrl Pts',(12.9470123424645,10.2789131332973,0.139042654788077));
#11018=CARTESIAN_POINT('Ctrl Pts',(13.1268055014811,11.2276337797824,0.0876844149673041));
#11019=CARTESIAN_POINT('Ctrl Pts',(13.9605773780345,11.8969878744382,0.0363261751465303));
#11020=CARTESIAN_POINT('Ctrl Pts',(14.6157705619694,12.0223122647246,-5.44540541130845E-16));
#11021=CARTESIAN_POINT('Origin',(15.,10.,9.54592528053767));
#11022=CARTESIAN_POINT('',(12.9464948772178,9.99822649168832,0.85407471946232));
#11023=CARTESIAN_POINT('',(12.9437809019177,10.0016640710788,0.795925280537675));
#11024=CARTESIAN_POINT('',(12.94525,10.0000000000001,9.54592528053767));
#11025=CARTESIAN_POINT('Ctrl Pts',(12.9437809019177,10.0016640710788,0.795925280537675));
#11026=CARTESIAN_POINT('Ctrl Pts',(12.9428201393579,10.1117045448354,0.789946197926163));
#11027=CARTESIAN_POINT('Ctrl Pts',(13.0009022569502,10.90254603781,0.746920066138311));
#11028=CARTESIAN_POINT('Ctrl Pts',(14.0270250684493,12.2251230724266,0.66684688517412));
#11029=CARTESIAN_POINT('Ctrl Pts',(16.3419551102441,12.024459772841,0.555705737645098));
#11030=CARTESIAN_POINT('Ctrl Pts',(17.4284073232916,9.96991710195404,0.444564590116078));
#11031=CARTESIAN_POINT('Ctrl Pts',(16.2921949921082,7.9444041673974,0.333423442587059));
#11032=CARTESIAN_POINT('Ctrl Pts',(13.9727677026847,7.79758395766853,0.222282295058038));
#11033=CARTESIAN_POINT('Ctrl Pts',(12.9909169312602,9.13320804851158,0.143116241041577));
#11034=CARTESIAN_POINT('Ctrl Pts',(12.9426893123183,9.90538408392121,0.100997236201456));
#11035=CARTESIAN_POINT('Ctrl Pts',(12.943442368457,9.99843416552646,0.0959252805376745));
#11036=CARTESIAN_POINT('Ctrl Pts',(12.9464948772178,9.99822649168832,0.85407471946232));
#11037=CARTESIAN_POINT('Ctrl Pts',(12.9504642873018,10.4798921519117,0.827991616512784));
#11038=CARTESIAN_POINT('Ctrl Pts',(13.3599168531639,11.6517645344229,0.764861464386909));
#11039=CARTESIAN_POINT('Ctrl Pts',(15.3128190766481,12.4084404416678,0.664684263084692));
#11040=CARTESIAN_POINT('Ctrl Pts',(17.1931639076296,11.0432447117585,0.553543115555672));
#11041=CARTESIAN_POINT('Ctrl Pts',(17.0658793839574,8.72328862566383,0.442401968026654));
#11042=CARTESIAN_POINT('Ctrl Pts',(15.0477523711852,7.57162591137588,0.331260820497632));
#11043=CARTESIAN_POINT('Ctrl Pts',(13.2644776059679,8.49852188099848,0.235151737642855));
#11044=CARTESIAN_POINT('Ctrl Pts',(12.9499854370273,9.59354193643066,0.176089703964417));
#11045=CARTESIAN_POINT('Ctrl Pts',(12.9482186935975,10.0008196174515,0.15407471946232));
#11046=CARTESIAN_POINT('Origin',(15.,10.,9.54592528053767));
#11047=CARTESIAN_POINT('',(12.9418691959132,10.000029918806,1.55407471946232));
#11048=CARTESIAN_POINT('',(12.9485192215913,10.0004498942776,1.49592528053768));
#11049=CARTESIAN_POINT('',(12.94525,10.0000000000001,9.54592528053767));
#11050=CARTESIAN_POINT('Ctrl Pts',(12.9485192215913,10.0004498942776,1.49592528053768));
#11051=CARTESIAN_POINT('Ctrl Pts',(12.947902332727,10.3157203421523,1.47889515965087));
#11052=CARTESIAN_POINT('Ctrl Pts',(13.1644765824467,11.3160215182978,1.42481798958772));
#11053=CARTESIAN_POINT('Ctrl Pts',(14.7222622877187,12.4127108006303,1.33369377034824));
#11054=CARTESIAN_POINT('Ctrl Pts',(16.8764722993871,11.541813251237,1.22255262281922));
#11055=CARTESIAN_POINT('Ctrl Pts',(17.3130317733822,9.25958632559344,1.1114114752902));
#11056=CARTESIAN_POINT('Ctrl Pts',(15.6323372531142,7.65513288048749,1.00027032776118));
#11057=CARTESIAN_POINT('Ctrl Pts',(13.4943745301596,8.16787145671535,0.895108262843671));
#11058=CARTESIAN_POINT('Ctrl Pts',(12.9487731291581,9.42988174566537,0.826993247102503));
#11059=CARTESIAN_POINT('Ctrl Pts',(12.9437809019177,10.0016640710788,0.795925280537675));
#11060=CARTESIAN_POINT('Ctrl Pts',(12.9418691959133,10.000029918806,1.55407471946232));
#11061=CARTESIAN_POINT('Ctrl Pts',(12.9418688527435,10.0016288743128,1.55398762741383));
#11062=CARTESIAN_POINT('Ctrl Pts',(12.9425946663912,10.6833881469544,1.516853486189));
#11063=CARTESIAN_POINT('Ctrl Pts',(13.6876865240177,12.0435635368564,1.44267229578783));
#11064=CARTESIAN_POINT('Ctrl Pts',(16.0052515541106,12.2108349221453,1.33153114825881));
#11065=CARTESIAN_POINT('Ctrl Pts',(17.402649969509,10.3543936274306,1.22039000072979));
#11066=CARTESIAN_POINT('Ctrl Pts',(16.6007558214423,8.1735579042694,1.10924885320077));
#11067=CARTESIAN_POINT('Ctrl Pts',(14.333596515509,7.6645683089416,0.998107705671753));
#11068=CARTESIAN_POINT('Ctrl Pts',(13.0653412380888,8.91110299629741,0.913049661092268));
#11069=CARTESIAN_POINT('Ctrl Pts',(12.9448263487916,9.79575992134947,0.865038665689124));
#11070=CARTESIAN_POINT('Ctrl Pts',(12.9464948772178,9.99822649168832,0.85407471946232));
#11071=CARTESIAN_POINT('Origin',(15.,10.,9.54592528053767));
#11072=CARTESIAN_POINT('',(12.9465817778743,10.0017541282055,2.25407471946232));
#11073=CARTESIAN_POINT('',(12.9454276661632,9.99812063713314,2.19592528053768));
#11074=CARTESIAN_POINT('',(12.94525,10.0000000000001,9.54592528053767));
#11075=CARTESIAN_POINT('Ctrl Pts',(12.9454276661632,9.99812063713314,2.19592528053768));
#11076=CARTESIAN_POINT('Ctrl Pts',(12.9501502076194,10.516002250193,2.16784412137558));
#11077=CARTESIAN_POINT('Ctrl Pts',(13.4114067040829,11.7246096284375,2.10271591303714));
#11078=CARTESIAN_POINT('Ctrl Pts',(15.4418987717874,12.3881053056886,2.00054065552236));
#11079=CARTESIAN_POINT('Ctrl Pts',(17.2460700947607,10.9238457607613,1.88939950799334));
#11080=CARTESIAN_POINT('Ctrl Pts',(16.9942776158352,8.61393405853105,1.77825836046432));
#11081=CARTESIAN_POINT('Ctrl Pts',(14.9170023251788,7.57277284889803,1.6671172129353));
#11082=CARTESIAN_POINT('Ctrl Pts',(13.2223586190082,8.57249152911901,1.57300618629308));
#11083=CARTESIAN_POINT('Ctrl Pts',(12.9492443027719,9.62988611561382,1.51594220882721));
#11084=CARTESIAN_POINT('Ctrl Pts',(12.9485192215913,10.0004498942776,1.49592528053768));
#11085=CARTESIAN_POINT('Ctrl Pts',(12.9465817778743,10.0017541282055,2.25407471946232));
#11086=CARTESIAN_POINT('Ctrl Pts',(12.9449103696296,10.2074604401693,2.24293658913854));
#11087=CARTESIAN_POINT('Ctrl Pts',(13.067863149555,11.095423500733,2.19475140963841));
#11088=CARTESIAN_POINT('Ctrl Pts',(14.3445560622211,12.3385280047513,2.10951918096195));
#11089=CARTESIAN_POINT('Ctrl Pts',(16.6093059338468,11.8189157324019,1.99837803343293));
#11090=CARTESIAN_POINT('Ctrl Pts',(17.4009607961183,9.63433987693309,1.88723688590391));
#11091=CARTESIAN_POINT('Ctrl Pts',(15.9948710360845,7.78447490731078,1.77609573837489));
#11092=CARTESIAN_POINT('Ctrl Pts',(13.6799311754379,7.96247429466911,1.66504168289436));
#11093=CARTESIAN_POINT('Ctrl Pts',(12.9420148296229,9.32146823602665,1.59103467659017));
#11094=CARTESIAN_POINT('Ctrl Pts',(12.9418691959133,10.000029918806,1.55407471946232));
#11095=CARTESIAN_POINT('Origin',(15.,10.,9.54592528053767));
#11096=CARTESIAN_POINT('',(12.9480745221571,9.99894822631912,2.95407471946232));
#11097=CARTESIAN_POINT('',(12.9421553640983,10.0006952919847,2.89592528053768));
#11098=CARTESIAN_POINT('',(12.94525,10.0000000000001,9.54592528053767));
#11099=CARTESIAN_POINT('Ctrl Pts',(12.9421553640983,10.0006952919847,2.89592528053768));
#11100=CARTESIAN_POINT('Ctrl Pts',(12.941987013991,10.0389915845278,2.89384013227662));
#11101=CARTESIAN_POINT('Ctrl Pts',(12.9603124687549,10.7575378196829,2.85470793483923));
#11102=CARTESIAN_POINT('Ctrl Pts',(13.79948312919,12.1111799816138,2.77852868822549));
#11103=CARTESIAN_POINT('Ctrl Pts',(16.1226906277949,12.1535754969733,2.66738754069648));
#11104=CARTESIAN_POINT('Ctrl Pts',(17.4182315125643,10.2246731484105,2.55624639316745));
#11105=CARTESIAN_POINT('Ctrl Pts',(16.5002188767733,8.09011387728591,2.44510524563844));
#11106=CARTESIAN_POINT('Ctrl Pts',(14.208965194919,7.70378886396441,2.33396409810942));
#11107=CARTESIAN_POINT('Ctrl Pts',(13.0377584374779,8.9858737770289,2.2509041097425));
#11108=CARTESIAN_POINT('Ctrl Pts',(12.9439198300002,9.83276885958405,2.20489117055192));
#11109=CARTESIAN_POINT('Ctrl Pts',(12.9454276661632,9.99812063713314,2.19592528053768));
#11110=CARTESIAN_POINT('Ctrl Pts',(12.9480745221571,9.99894822631912,2.95407471946232));
#11111=CARTESIAN_POINT('Ctrl Pts',(12.9499783117173,10.4095028651207,2.93188555086324));
#11112=CARTESIAN_POINT('Ctrl Pts',(13.2684548594827,11.5082393253183,2.87264933308783));
#11113=CARTESIAN_POINT('Ctrl Pts',(15.0590413979142,12.4279279486728,2.77636606613607));
#11114=CARTESIAN_POINT('Ctrl Pts',(17.071896801884,11.2671083826901,2.66522491860705));
#11115=CARTESIAN_POINT('Ctrl Pts',(17.1882197878565,8.94642789870889,2.55408377107803));
#11116=CARTESIAN_POINT('Ctrl Pts',(15.3015328924376,7.59014566366572,2.44294262354901));
#11117=CARTESIAN_POINT('Ctrl Pts',(13.3555718476664,8.35460491178446,2.34293960634377));
#11118=CARTESIAN_POINT('Ctrl Pts',(12.9504697177102,9.52325118478529,2.27998363831488));
#11119=CARTESIAN_POINT('Ctrl Pts',(12.9465817778743,10.0017541282055,2.25407471946232));
#11120=CARTESIAN_POINT('Origin',(15.,10.,9.54592528053767));
#11121=CARTESIAN_POINT('',(12.9427436128433,9.99880853413039,3.65407471946232));
#11122=CARTESIAN_POINT('',(12.9474825844755,10.0014423099628,3.59592528053768));
#11123=CARTESIAN_POINT('',(12.94525,10.0000000000001,9.54592528053767));
#11124=CARTESIAN_POINT('Ctrl Pts',(12.9474825844755,10.0014423099628,3.59592528053768));
#11125=CARTESIAN_POINT('Ctrl Pts',(12.9459094100193,10.2443186941233,3.58278909400133));
#11126=CARTESIAN_POINT('Ctrl Pts',(13.0981153059447,11.1702543569017,3.53260585828864));
#11127=CARTESIAN_POINT('Ctrl Pts',(14.4712648228307,12.3703925377072,3.44537557339962));
#11128=CARTESIAN_POINT('Ctrl Pts',(16.7047942952545,11.7297393101775,3.33423442587059));
#11129=CARTESIAN_POINT('Ctrl Pts',(17.3778224702348,9.50575110480829,3.22309327834158));
#11130=CARTESIAN_POINT('Ctrl Pts',(15.8742859650895,7.73417879746959,3.11195213081255));
#11131=CARTESIAN_POINT('Ctrl Pts',(13.6136852874083,8.03097490314885,3.00289613154459));
#11132=CARTESIAN_POINT('Ctrl Pts',(12.9449781081118,9.35857731393861,2.93088718145296));
#11133=CARTESIAN_POINT('Ctrl Pts',(12.9421553640983,10.0006952919847,2.89592528053768));
#11134=CARTESIAN_POINT('Ctrl Pts',(12.9427436128433,9.99880853413039,3.65407471946232));
#11135=CARTESIAN_POINT('Ctrl Pts',(12.9469605443102,10.6097671110138,3.62083451258795));
#11136=CARTESIAN_POINT('Ctrl Pts',(13.5593536683009,11.9089948024551,3.55054725653724));
#11137=CARTESIAN_POINT('Ctrl Pts',(15.7683368037833,12.3039050690097,3.44321295131019));
#11138=CARTESIAN_POINT('Ctrl Pts',(17.3523611503097,10.6039180652812,3.33207180378117));
#11139=CARTESIAN_POINT('Ctrl Pts',(16.7831271023553,8.35112834097283,3.22093065625215));
#11140=CARTESIAN_POINT('Ctrl Pts',(14.5816890022697,7.60765054388266,3.10978950872313));
#11141=CARTESIAN_POINT('Ctrl Pts',(13.1262236723966,8.76526632942327,3.02083752979318));
#11142=CARTESIAN_POINT('Ctrl Pts',(12.9467997435279,9.72404059440326,2.96893260003958));
#11143=CARTESIAN_POINT('Ctrl Pts',(12.9480745221571,9.99894822631912,2.95407471946232));
#11144=CARTESIAN_POINT('Origin',(15.,10.,9.54592528053767));
#11145=CARTESIAN_POINT('',(12.944465687196,10.0018026581102,4.35407471946232));
#11146=CARTESIAN_POINT('',(12.9473703407886,9.99850463442125,4.29592528053768));
#11147=CARTESIAN_POINT('',(12.94525,10.0000000000001,9.54592528053767));
#11148=CARTESIAN_POINT('Ctrl Pts',(12.9473703407886,9.99850463442125,4.29592528053768));
#11149=CARTESIAN_POINT('Ctrl Pts',(12.9503841045655,10.4456433922625,4.27173805572604));
#11150=CARTESIAN_POINT('Ctrl Pts',(13.3139391530161,11.5821159767798,4.21050378173806));
#11151=CARTESIAN_POINT('Ctrl Pts',(15.1895240703454,12.4212398264365,4.11222245857373));
#11152=CARTESIAN_POINT('Ctrl Pts',(17.1370409604027,11.1538533719331,4.00108131104472));
#11153=CARTESIAN_POINT('Ctrl Pts',(17.1283950449557,8.83027515929254,3.88994016351569));
#11154=CARTESIAN_POINT('Ctrl Pts',(15.1715004531809,7.57741681981306,3.77879901598667));
#11155=CARTESIAN_POINT('Ctrl Pts',(13.3074684046186,8.42807639372317,3.680794054994));
#11156=CARTESIAN_POINT('Ctrl Pts',(12.9503461216389,9.55935176533709,3.61983614317767));
#11157=CARTESIAN_POINT('Ctrl Pts',(12.9474825844755,10.0014423099628,3.59592528053768));
#11158=CARTESIAN_POINT('Ctrl Pts',(12.944465687196,10.0018026581102,4.35407471946232));
#11159=CARTESIAN_POINT('Ctrl Pts',(12.9432417525907,10.1352420818974,4.346830523489));
#11160=CARTESIAN_POINT('Ctrl Pts',(13.0158868434944,10.9497682245499,4.30253927833933));
#11161=CARTESIAN_POINT('Ctrl Pts',(14.1033972467191,12.2570829656611,4.22120098401333));
#11162=CARTESIAN_POINT('Ctrl Pts',(16.4100928881365,11.9773613877815,4.11005983648431));
#11163=CARTESIAN_POINT('Ctrl Pts',(17.4260452489189,9.88764137211515,3.99891868895528));
#11164=CARTESIAN_POINT('Ctrl Pts',(16.2212917045089,7.90077000222407,3.88777754142627));
#11165=CARTESIAN_POINT('Ctrl Pts',(13.8986160185493,7.83545077753679,3.77663639389725));
#11166=CARTESIAN_POINT('Ctrl Pts',(12.9772493640344,9.17842806969361,3.6987354532426));
#11167=CARTESIAN_POINT('Ctrl Pts',(12.9422606678017,9.92883836324606,3.65788156176429));
#11168=CARTESIAN_POINT('Ctrl Pts',(12.9427436128433,9.99880853413039,3.65407471946232));
#11169=CARTESIAN_POINT('Origin',(15.,10.,9.54592528053767));
#11170=CARTESIAN_POINT('',(12.9486078680663,10.0000693726643,5.05407471946232));
#11171=CARTESIAN_POINT('',(12.9420873152149,9.99939266312408,4.99592528053768));
#11172=CARTESIAN_POINT('',(12.94525,10.0000000000001,9.54592528053767));
#11173=CARTESIAN_POINT('Ctrl Pts',(12.9420873152149,9.99939266312408,4.99592528053768));
#11174=CARTESIAN_POINT('Ctrl Pts',(12.9446118235547,10.6465293223607,4.96068701745075));
#11175=CARTESIAN_POINT('Ctrl Pts',(13.6226426588603,11.9785777748891,4.88840170518747));
#11176=CARTESIAN_POINT('Ctrl Pts',(15.8911235313356,12.2592522042247,4.77906934374785));
#11177=CARTESIAN_POINT('Ctrl Pts',(17.381434725746,10.4765399430985,4.66792819621883));
#11178=CARTESIAN_POINT('Ctrl Pts',(16.6918747241627,8.25762185846654,4.55678704868982));
#11179=CARTESIAN_POINT('Ctrl Pts',(14.4536394897207,7.63360783825394,4.44564590116079));
#11180=CARTESIAN_POINT('Ctrl Pts',(13.0937811610426,8.84009694702206,4.35869197844341));
#11181=CARTESIAN_POINT('Ctrl Pts',(12.9457679877634,9.76077062660234,4.30878510490238));
#11182=CARTESIAN_POINT('Ctrl Pts',(12.9473703407886,9.99850463442125,4.29592528053768));
#11183=CARTESIAN_POINT('Ctrl Pts',(12.9486078680663,10.0000693726643,5.05407471946232));
#11184=CARTESIAN_POINT('Ctrl Pts',(12.9485058673419,10.3387965081927,5.0357794852137));
#11185=CARTESIAN_POINT('Ctrl Pts',(13.1882324475917,11.36329538309,4.98043720178874));
#11186=CARTESIAN_POINT('Ctrl Pts',(14.8046014881481,12.4207724868025,4.88804786918745));
#11187=CARTESIAN_POINT('Ctrl Pts',(16.9278971892049,11.4770011641531,4.77690672165842));
#11188=CARTESIAN_POINT('Ctrl Pts',(17.2864720241886,9.18124137035986,4.66576557412941));
#11189=CARTESIAN_POINT('Ctrl Pts',(15.5521007657847,7.63494085580992,4.55462442660038));
#11190=CARTESIAN_POINT('Ctrl Pts',(13.4583450304019,8.21320277091433,4.45072747504469));
#11191=CARTESIAN_POINT('Ctrl Pts',(12.9495009931851,9.45282861416286,4.38387757266534));
#11192=CARTESIAN_POINT('Ctrl Pts',(12.944465687196,10.0018026581102,4.35407471946232));
#11193=CARTESIAN_POINT('Origin',(15.,10.,9.54592528053767));
#11194=CARTESIAN_POINT('',(12.9447203589281,9.99816149350058,5.75407471946233));
#11195=CARTESIAN_POINT('',(12.9455805553419,10.0018769103914,5.69592528053768));
#11196=CARTESIAN_POINT('',(12.94525,10.0000000000001,9.54592528053767));
#11197=CARTESIAN_POINT('Ctrl Pts',(12.9455805553419,10.0018769103914,5.69592528053768));
#11198=CARTESIAN_POINT('Ctrl Pts',(12.9440383474063,10.172357811441,5.68668302835179));
#11199=CARTESIAN_POINT('Ctrl Pts',(13.0414311459384,11.024464022361,5.64039372698956));
#11200=CARTESIAN_POINT('Ctrl Pts',(14.2260750296995,12.3020342758629,5.55705737645099));
#11201=CARTESIAN_POINT('Ctrl Pts',(16.51439031526,11.8986689139798,5.44591622892198));
#11202=CARTESIAN_POINT('Ctrl Pts',(17.4164925788533,9.75733709227475,5.33477508139295));
#11203=CARTESIAN_POINT('Ctrl Pts',(16.1066330737735,7.83812930313874,5.22363393386394));
#11204=CARTESIAN_POINT('Ctrl Pts',(13.7838054045903,7.89781247823008,5.11249278633491));
#11205=CARTESIAN_POINT('Ctrl Pts',(12.9577392125388,9.25272884593619,5.03658990189283));
#11206=CARTESIAN_POINT('Ctrl Pts',(12.9419577317687,9.96617502738866,4.99773406662709));
#11207=CARTESIAN_POINT('Ctrl Pts',(12.9420873152149,9.99939266312408,4.99592528053768));
#11208=CARTESIAN_POINT('Ctrl Pts',(12.9447203589281,9.99816149350058,5.75407471946233));
#11209=CARTESIAN_POINT('Ctrl Pts',(12.9497104259152,10.538897567902,5.72472844693841));
#11210=CARTESIAN_POINT('Ctrl Pts',(13.445663016072,11.770362488044,5.65833512523815));
#11211=CARTESIAN_POINT('Ctrl Pts',(15.5229818972268,12.3716681799822,5.55489475436157));
#11212=CARTESIAN_POINT('Ctrl Pts',(17.2762330137476,10.8468076994282,5.44375360683255));
#11213=CARTESIAN_POINT('Ctrl Pts',(16.9459104193154,8.54681293441946,5.33261245930352));
#11214=CARTESIAN_POINT('Ctrl Pts',(14.8343783616792,7.57700815405708,5.22147131177451));
#11215=CARTESIAN_POINT('Ctrl Pts',(13.1970787562676,8.61966030426231,5.12862539849411));
#11216=CARTESIAN_POINT('Ctrl Pts',(12.9487124143475,9.65288887362781,5.07282653439004));
#11217=CARTESIAN_POINT('Ctrl Pts',(12.9486078680663,10.0000693726643,5.05407471946232));
#11218=CARTESIAN_POINT('Origin',(15.,10.,9.54592528053767));
#11219=CARTESIAN_POINT('',(12.9425629288878,10.0010699703231,6.45407471946232));
#11220=CARTESIAN_POINT('',(12.9484827731942,9.99946914088102,6.39592528053768));
#11221=CARTESIAN_POINT('',(12.94525,10.0000000000001,9.54592528053767));
#11222=CARTESIAN_POINT('Ctrl Pts',(12.9484827731942,9.99946914088102,6.39592528053768));
#11223=CARTESIAN_POINT('Ctrl Pts',(12.9493514564268,10.3751323293684,6.3756319900765));
#11224=CARTESIAN_POINT('Ctrl Pts',(13.2280330016817,11.4377987966319,6.31829165043898));
#11225=CARTESIAN_POINT('Ctrl Pts',(14.9350675106875,12.4277778414421,6.22390426162511));
#11226=CARTESIAN_POINT('Ctrl Pts',(17.0045372308406,11.3711864275124,6.1127631140961));
#11227=CARTESIAN_POINT('Ctrl Pts',(17.2391328194089,9.05946509552617,6.00162196656707));
#11228=CARTESIAN_POINT('Ctrl Pts',(15.424114751786,7.608672268086,5.89048081903805));
#11229=CARTESIAN_POINT('Ctrl Pts',(13.4040950392535,8.28542469052011,5.78858192369492));
#11230=CARTESIAN_POINT('Ctrl Pts',(12.9502202013615,9.48899468762855,5.72373007752813));
#11231=CARTESIAN_POINT('Ctrl Pts',(12.9455805553419,10.0018769103914,5.69592528053768));
#11232=CARTESIAN_POINT('Ctrl Pts',(12.9425629288878,10.0010699703231,6.45407471946232));
#11233=CARTESIAN_POINT('Ctrl Pts',(12.9421730677846,10.0626339108422,6.45072445783945));
#11234=CARTESIAN_POINT('Ctrl Pts',(12.9726042727645,10.8045784977884,6.41032714704025));
#11235=CARTESIAN_POINT('Ctrl Pts',(13.8720874462699,12.1508444526632,6.33288278706471));
#11236=CARTESIAN_POINT('Ctrl Pts',(16.1953904039119,12.1140865945272,6.22174163953568));
#11237=CARTESIAN_POINT('Ctrl Pts',(17.4244805427636,10.1421770013196,6.11060049200667));
#11238=CARTESIAN_POINT('Ctrl Pts',(16.4342968937075,8.04012443367538,5.99945934447764));
#11239=CARTESIAN_POINT('Ctrl Pts',(14.1312146531314,7.73206435471271,5.88831819694863));
#11240=CARTESIAN_POINT('Ctrl Pts',(13.0215193522343,9.03317276281873,5.80652332194352));
#11241=CARTESIAN_POINT('Ctrl Pts',(12.9434109118316,9.85626654812099,5.76177549611475));
#11242=CARTESIAN_POINT('Ctrl Pts',(12.9447203589281,9.99816149350058,5.75407471946233));
#11243=CARTESIAN_POINT('Origin',(15.,10.,9.54592528053767));
#11244=CARTESIAN_POINT('',(12.9479405474349,10.0011587877502,7.15407471946232));
#11245=CARTESIAN_POINT('',(12.9436341942584,9.99839713117394,7.09592528053768));
#11246=CARTESIAN_POINT('',(12.94525,10.0000000000001,9.54592528053767));
#11247=CARTESIAN_POINT('Ctrl Pts',(12.9436341942584,9.99839713117394,7.09592528053768));
#11248=CARTESIAN_POINT('Ctrl Pts',(12.9485802607195,10.5751617788476,7.0645809518012));
#11249=CARTESIAN_POINT('Ctrl Pts',(13.5024258197495,11.8419530434235,6.99618957388839));
#11250=CARTESIAN_POINT('Ctrl Pts',(15.6497677286939,12.3401097288481,6.89075114679923));
#11251=CARTESIAN_POINT('Ctrl Pts',(17.3184787798211,10.7231732227644,6.77960999927021));
#11252=CARTESIAN_POINT('Ctrl Pts',(16.864945940343,8.44426865073882,6.66846885174118));
#11253=CARTESIAN_POINT('Ctrl Pts',(14.7043153597183,7.58942105489702,6.55732770421218));
#11254=CARTESIAN_POINT('Ctrl Pts',(13.1594333615178,8.69431383299048,6.46647984714433));
#11255=CARTESIAN_POINT('Ctrl Pts',(12.9477656046647,9.68932868188927,6.41267903925283));
#11256=CARTESIAN_POINT('Ctrl Pts',(12.9484827731942,9.99946914088102,6.39592528053768));
#11257=CARTESIAN_POINT('Ctrl Pts',(12.9479405474349,10.0011587877502,7.15407471946232));
#11258=CARTESIAN_POINT('Ctrl Pts',(12.9465638731556,10.2675785025657,7.13967341956416));
#11259=CARTESIAN_POINT('Ctrl Pts',(13.1185705249126,11.2176540004845,7.08822507048966));
#11260=CARTESIAN_POINT('Ctrl Pts',(14.552316547407,12.3870127270114,6.99972967223883));
#11261=CARTESIAN_POINT('Ctrl Pts',(16.7627159052523,11.6706763447836,6.8885885247098));
#11262=CARTESIAN_POINT('Ctrl Pts',(17.359610496679,9.42504513942049,6.77744737718079));
#11263=CARTESIAN_POINT('Ctrl Pts',(15.796602835303,7.70571713781293,6.66630622965176));
#11264=CARTESIAN_POINT('Ctrl Pts',(13.5735166221464,8.07500088427441,6.55851534374561));
#11265=CARTESIAN_POINT('Ctrl Pts',(12.9464841351245,9.38186249993724,6.48777150701579));
#11266=CARTESIAN_POINT('Ctrl Pts',(12.9425629288878,10.0010699703231,6.45407471946232));
#11267=CARTESIAN_POINT('Origin',(15.,10.,9.54592528053767));
#11268=CARTESIAN_POINT('',(12.9473113968994,9.99752941021421,7.85407471946233));
#11269=CARTESIAN_POINT('',(12.9434528818545,10.0014882284141,7.79592528053768));
#11270=CARTESIAN_POINT('',(12.94525,10.0000000000001,9.54592528053767));
#11271=CARTESIAN_POINT('',(14.4698297828114,8.01482567432828,8.));
#11272=CARTESIAN_POINT('Ctrl Pts',(14.4698297828114,8.01482567432828,8.));
#11273=CARTESIAN_POINT('Ctrl Pts',(13.8096927451188,8.1911250512252,7.96295295082366));
#11274=CARTESIAN_POINT('Ctrl Pts',(13.0749952948832,8.88701044345236,7.91431119064444));
#11275=CARTESIAN_POINT('Ctrl Pts',(12.9456877182649,9.7832841399949,7.86566943046521));
#11276=CARTESIAN_POINT('Ctrl Pts',(12.9473113968994,9.99752941021421,7.85407471946233));
#11277=CARTESIAN_POINT('',(15.5312698928193,8.01125028009066,8.));
#11278=CARTESIAN_POINT('Origin',(15.,10.,8.));
#11279=CARTESIAN_POINT('Ctrl Pts',(15.531270276981,8.01124903105919,8.));
#11280=CARTESIAN_POINT('Ctrl Pts',(14.8865857166431,7.83988501971335,7.96367382485347));
#11281=CARTESIAN_POINT('Ctrl Pts',(13.5069335921707,8.15949860066886,7.89564891836603));
#11282=CARTESIAN_POINT('Ctrl Pts',(12.9483221305924,9.41848319233778,7.82762401187859));
#11283=CARTESIAN_POINT('Ctrl Pts',(12.9434528818545,10.0014882284141,7.79592528053768));
#11284=CARTESIAN_POINT('Origin',(-15.,-10.,9.54592528053767));
#11285=CARTESIAN_POINT('',(-17.0517816873057,-9.99918029423424,0.15407471946232));
#11286=CARTESIAN_POINT('',(-17.0565583212302,-10.0015648221723,0.0959252805376758));
#11287=CARTESIAN_POINT('',(-17.05475,-9.99999999999991,9.54592528053767));
#11288=CARTESIAN_POINT('',(-16.3390017195986,-8.44145197141315,1.11022302462516E-15));
#11289=CARTESIAN_POINT('Ctrl Pts',(-17.0565583212302,-10.0015648221723,
0.0959252805376758));
#11290=CARTESIAN_POINT('Ctrl Pts',(-17.0518107016117,-9.41495008139905,
0.0639501870251164));
#11291=CARTESIAN_POINT('Ctrl Pts',(-16.7863171109465,-8.82575586659747,
0.0319750935125572));
#11292=CARTESIAN_POINT('Ctrl Pts',(-16.3390017195986,-8.44145197141311,
-2.22044604925031E-15));
#11293=CARTESIAN_POINT('',(-15.3842288288255,-7.97768903459251,4.89463757827447E-16));
#11294=CARTESIAN_POINT('Origin',(-15.,-10.,0.));
#11295=CARTESIAN_POINT('Ctrl Pts',(-17.0517816873057,-9.99918029423424,
0.15407471946232));
#11296=CARTESIAN_POINT('Ctrl Pts',(-17.0529881094183,-9.72108671039038,
0.139042654788077));
#11297=CARTESIAN_POINT('Ctrl Pts',(-16.8731950448097,-8.77236588328783,
0.0876844149673042));
#11298=CARTESIAN_POINT('Ctrl Pts',(-16.0394219710344,-8.10301220682191,
0.0363261751465313));
#11299=CARTESIAN_POINT('Ctrl Pts',(-15.3842290239278,-7.97768774796568,
8.9812597463268E-16));
#11300=CARTESIAN_POINT('Origin',(-15.,-10.,9.54592528053767));
#11301=CARTESIAN_POINT('',(-17.0535052914424,-10.0017735080204,0.854074719462321));
#11302=CARTESIAN_POINT('',(-17.0562189577482,-9.9983358962701,0.795925280537676));
#11303=CARTESIAN_POINT('',(-17.05475,-9.99999999999991,9.54592528053767));
#11304=CARTESIAN_POINT('Ctrl Pts',(-17.0562189577482,-9.9983358962701,0.795925280537676));
#11305=CARTESIAN_POINT('Ctrl Pts',(-17.0571797200526,-9.88829543020703,
0.789946197926163));
#11306=CARTESIAN_POINT('Ctrl Pts',(-16.9990976027996,-9.09745400255305,
0.74692006613831));
#11307=CARTESIAN_POINT('Ctrl Pts',(-15.9729748140483,-7.77487725906727,
0.666846885174117));
#11308=CARTESIAN_POINT('Ctrl Pts',(-13.6580450846071,-7.97554008402429,
0.555705737645098));
#11309=CARTESIAN_POINT('Ctrl Pts',(-12.5715926480149,-10.0300833696701,
0.444564590116077));
#11310=CARTESIAN_POINT('Ctrl Pts',(-13.7078055175393,-12.0555949236832,
0.333423442587058));
#11311=CARTESIAN_POINT('Ctrl Pts',(-16.0272313718098,-12.2024171088693,
0.222282295058038));
#11312=CARTESIAN_POINT('Ctrl Pts',(-17.0090838666329,-10.8667907385836,
0.143116241041577));
#11313=CARTESIAN_POINT('Ctrl Pts',(-17.0573113985028,-10.0946148692583,
0.100997236201457));
#11314=CARTESIAN_POINT('Ctrl Pts',(-17.0565583212302,-10.0015648221723,
0.0959252805376758));
#11315=CARTESIAN_POINT('Ctrl Pts',(-17.0535052914424,-10.0017735080204,
0.854074719462321));
#11316=CARTESIAN_POINT('Ctrl Pts',(-17.0495358857753,-9.52010780339371,
0.827991616512785));
#11317=CARTESIAN_POINT('Ctrl Pts',(-16.6400833000123,-8.34823531025937,
0.764861464386909));
#11318=CARTESIAN_POINT('Ctrl Pts',(-14.687180849695,-7.59155940883828,0.664684263084691));
#11319=CARTESIAN_POINT('Ctrl Pts',(-12.8068360000695,-8.95675512341312,
0.553543115555673));
#11320=CARTESIAN_POINT('Ctrl Pts',(-12.9341202906761,-11.2767116091318,
0.442401968026652));
#11321=CARTESIAN_POINT('Ctrl Pts',(-14.9522479049698,-12.4283740802081,
0.331260820497633));
#11322=CARTESIAN_POINT('Ctrl Pts',(-16.7355221426696,-11.5014784845208,
0.235151737642855));
#11323=CARTESIAN_POINT('Ctrl Pts',(-17.050014839924,-10.4064580748405,0.176089703964417));
#11324=CARTESIAN_POINT('Ctrl Pts',(-17.0517816873057,-9.99918029423424,
0.15407471946232));
#11325=CARTESIAN_POINT('Origin',(-15.,-10.,9.54592528053767));
#11326=CARTESIAN_POINT('',(-17.0581309722196,-9.99997008132667,1.55407471946232));
#11327=CARTESIAN_POINT('',(-17.0514806312403,-9.99955010506969,1.49592528053768));
#11328=CARTESIAN_POINT('',(-17.05475,-9.99999999999991,9.54592528053767));
#11329=CARTESIAN_POINT('Ctrl Pts',(-17.0514806312403,-9.99955010506969,
1.49592528053768));
#11330=CARTESIAN_POINT('Ctrl Pts',(-17.0520975200814,-9.6842796794923,1.47889515965087));
#11331=CARTESIAN_POINT('Ctrl Pts',(-16.8355232859291,-8.68397857454396,
1.42481798958773));
#11332=CARTESIAN_POINT('Ctrl Pts',(-15.2777376918069,-7.58728937837554,
1.33369377034824));
#11333=CARTESIAN_POINT('Ctrl Pts',(-13.1235278364479,-8.45818684891592,
1.22255262281922));
#11334=CARTESIAN_POINT('Ctrl Pts',(-12.686968390135,-10.7404136399833,1.1114114752902));
#11335=CARTESIAN_POINT('Ctrl Pts',(-14.367662797513,-12.344866918125,1.00027032776118));
#11336=CARTESIAN_POINT('Ctrl Pts',(-16.5056253516517,-11.8321284649118,
0.895108262843669));
#11337=CARTESIAN_POINT('Ctrl Pts',(-17.0512267318348,-10.5701181817067,
0.826993247102503));
#11338=CARTESIAN_POINT('Ctrl Pts',(-17.0562189577482,-9.9983358962701,0.795925280537676));
#11339=CARTESIAN_POINT('Ctrl Pts',(-17.0581309722196,-9.99997008132667,
1.55407471946232));
#11340=CARTESIAN_POINT('Ctrl Pts',(-17.0581313153895,-9.99837112568893,
1.55398762741383));
#11341=CARTESIAN_POINT('Ctrl Pts',(-17.0574055017633,-9.31661179721689,
1.516853486189));
#11342=CARTESIAN_POINT('Ctrl Pts',(-16.3123135839388,-7.95643629520889,
1.44267229578783));
#11343=CARTESIAN_POINT('Ctrl Pts',(-13.9947483624482,-7.78916489875036,
1.33153114825881));
#11344=CARTESIAN_POINT('Ctrl Pts',(-12.5973498364434,-9.64560634071132,
1.22039000072979));
#11345=CARTESIAN_POINT('Ctrl Pts',(-13.3992440433914,-11.826442250177,1.10924885320077));
#11346=CARTESIAN_POINT('Ctrl Pts',(-15.6664035468934,-12.3354318728424,
0.998107705671752));
#11347=CARTESIAN_POINT('Ctrl Pts',(-16.934658910805,-11.0888971028013,0.913049661092267));
#11348=CARTESIAN_POINT('Ctrl Pts',(-17.0551738180119,-10.204240097024,0.865038665689124));
#11349=CARTESIAN_POINT('Ctrl Pts',(-17.0535052914424,-10.0017735080204,
0.854074719462321));
#11350=CARTESIAN_POINT('Origin',(-15.,-10.,9.54592528053767));
#11351=CARTESIAN_POINT('',(-17.0534183899706,-9.99824587165492,2.25407471946232));
#11352=CARTESIAN_POINT('',(-17.0545721863858,-10.0018793627325,2.19592528053768));
#11353=CARTESIAN_POINT('',(-17.05475,-9.99999999999991,9.54592528053767));
#11354=CARTESIAN_POINT('Ctrl Pts',(-17.0545721863858,-10.0018793627325,
2.19592528053768));
#11355=CARTESIAN_POINT('Ctrl Pts',(-17.0498496452687,-9.48399778682363,
2.16784412137558));
#11356=CARTESIAN_POINT('Ctrl Pts',(-16.5885931819089,-8.27539049526638,
2.10271591303714));
#11357=CARTESIAN_POINT('Ctrl Pts',(-14.5581012599229,-7.61189486585896,
2.00054065552235));
#11358=CARTESIAN_POINT('Ctrl Pts',(-12.7539300664426,-9.07615430524727,
1.88939950799334));
#11359=CARTESIAN_POINT('Ctrl Pts',(-13.0057225272674,-11.3860658425327,
1.77825836046431));
#11360=CARTESIAN_POINT('Ctrl Pts',(-15.0829976689147,-12.4272269759234,
1.6671172129353));
#11361=CARTESIAN_POINT('Ctrl Pts',(-16.7776412533276,-11.4275083697971,
1.57300618629308));
#11362=CARTESIAN_POINT('Ctrl Pts',(-17.0507555500869,-10.3701138575256,
1.51594220882721));
#11363=CARTESIAN_POINT('Ctrl Pts',(-17.0514806312403,-9.99955010506969,
1.49592528053768));
#11364=CARTESIAN_POINT('Ctrl Pts',(-17.0534183899706,-9.99824587165492,
2.25407471946232));
#11365=CARTESIAN_POINT('Ctrl Pts',(-17.0550897983517,-9.79253954287702,
2.24293658913854));
#11366=CARTESIAN_POINT('Ctrl Pts',(-16.932137008376,-8.90457640973076,2.19475140963841));
#11367=CARTESIAN_POINT('Ctrl Pts',(-15.6554439913718,-7.66147180407228,
2.10951918096195));
#11368=CARTESIAN_POINT('Ctrl Pts',(-13.3906939345767,-8.18108411896286,
1.99837803343293));
#11369=CARTESIAN_POINT('Ctrl Pts',(-12.5990390076834,-10.3656601528754,
1.88723688590391));
#11370=CARTESIAN_POINT('Ctrl Pts',(-14.0051288824869,-12.2155252739355,
1.77609573837489));
#11371=CARTESIAN_POINT('Ctrl Pts',(-16.3200689326647,-12.0375258716092,
1.66504168289436));
#11372=CARTESIAN_POINT('Ctrl Pts',(-17.0579853384182,-10.6785318196738,
1.59103467659017));
#11373=CARTESIAN_POINT('Ctrl Pts',(-17.0581309722196,-9.99997008132667,
1.55407471946232));
#11374=CARTESIAN_POINT('Origin',(-15.,-10.,9.54592528053767));
#11375=CARTESIAN_POINT('',(-17.0519256455684,-10.0010517737669,2.95407471946232));
#11376=CARTESIAN_POINT('',(-17.0578444882157,-9.99930470806554,2.89592528053768));
#11377=CARTESIAN_POINT('',(-17.05475,-9.99999999999991,9.54592528053767));
#11378=CARTESIAN_POINT('Ctrl Pts',(-17.0578444882157,-9.99930470806554,
2.89592528053768));
#11379=CARTESIAN_POINT('Ctrl Pts',(-17.0580128383109,-9.96100841827086,
2.89384013227662));
#11380=CARTESIAN_POINT('Ctrl Pts',(-17.0396873848621,-9.24246223468361,
2.85470793483923));
#11381=CARTESIAN_POINT('Ctrl Pts',(-16.2005167846521,-7.88882016989784,
2.77852868822549));
#11382=CARTESIAN_POINT('Ctrl Pts',(-13.8773094527777,-7.84642465758702,
2.66738754069648));
#11383=CARTESIAN_POINT('Ctrl Pts',(-12.5817686609856,-9.7753268677064,2.55624639316746));
#11384=CARTESIAN_POINT('Ctrl Pts',(-13.4997812308935,-11.9098859856603,
2.44510524563844));
#11385=CARTESIAN_POINT('Ctrl Pts',(-15.7910347483105,-12.2962109712173,
2.33396409810941));
#11386=CARTESIAN_POINT('Ctrl Pts',(-16.962241421697,-11.0141261502186,2.2509041097425));
#11387=CARTESIAN_POINT('Ctrl Pts',(-17.0560800224405,-10.1672311284198,
2.20489117055192));
#11388=CARTESIAN_POINT('Ctrl Pts',(-17.0545721863858,-10.0018793627325,
2.19592528053768));
#11389=CARTESIAN_POINT('Ctrl Pts',(-17.0519256455684,-10.0010517737669,
2.95407471946232));
#11390=CARTESIAN_POINT('Ctrl Pts',(-17.0500218558526,-9.59049710140644,
2.93188555086324));
#11391=CARTESIAN_POINT('Ctrl Pts',(-16.7315452820547,-8.49176055139755,
2.87264933308782));
#11392=CARTESIAN_POINT('Ctrl Pts',(-14.9409585972601,-7.57207185286643,
2.77636606613607));
#11393=CARTESIAN_POINT('Ctrl Pts',(-12.9281030287572,-8.73289151373681,
2.66522491860704));
#11394=CARTESIAN_POINT('Ctrl Pts',(-12.8117800332785,-11.0535721874087,
2.55408377107803));
#11395=CARTESIAN_POINT('Ctrl Pts',(-14.6984670829124,-12.4098545333209,
2.442942623549));
#11396=CARTESIAN_POINT('Ctrl Pts',(-16.6444282867541,-11.6453952227051,
2.34293960634378));
#11397=CARTESIAN_POINT('Ctrl Pts',(-17.0495304498177,-10.4767488541872,
2.27998363831488));
#11398=CARTESIAN_POINT('Ctrl Pts',(-17.0534183899706,-9.99824587165492,
2.25407471946232));
#11399=CARTESIAN_POINT('Origin',(-15.,-10.,9.54592528053767));
#11400=CARTESIAN_POINT('',(-17.057256555318,-10.001191465967,3.65407471946232));
#11401=CARTESIAN_POINT('',(-17.0525172682208,-9.99855769014068,3.59592528053768));
#11402=CARTESIAN_POINT('',(-17.05475,-9.99999999999991,9.54592528053767));
#11403=CARTESIAN_POINT('Ctrl Pts',(-17.0525172682208,-9.99855769014068,
3.59592528053768));
#11404=CARTESIAN_POINT('Ctrl Pts',(-17.0540904425641,-9.75568132341078,
3.58278909400133));
#11405=CARTESIAN_POINT('Ctrl Pts',(-16.901884557562,-8.82974572708431,3.53260585828864));
#11406=CARTESIAN_POINT('Ctrl Pts',(-15.5287351392234,-7.62960763240948,
3.44537557339961));
#11407=CARTESIAN_POINT('Ctrl Pts',(-13.2952058270941,-8.27026081396139,
3.33423442587059));
#11408=CARTESIAN_POINT('Ctrl Pts',(-12.6221777004152,-10.4942488597207,
3.22309327834158));
#11409=CARTESIAN_POINT('Ctrl Pts',(-14.1257140976557,-12.2658210399188,
3.11195213081255));
#11410=CARTESIAN_POINT('Ctrl Pts',(-16.3863146130996,-11.9690249555389,
3.00289613154459));
#11411=CARTESIAN_POINT('Ctrl Pts',(-17.0550217444047,-10.6414226400287,
2.93088718145296));
#11412=CARTESIAN_POINT('Ctrl Pts',(-17.0578444882157,-9.99930470806554,
2.89592528053768));
#11413=CARTESIAN_POINT('Ctrl Pts',(-17.057256555318,-10.001191465967,3.65407471946232));
#11414=CARTESIAN_POINT('Ctrl Pts',(-17.0530396235064,-9.39023283914347,
3.62083451258795));
#11415=CARTESIAN_POINT('Ctrl Pts',(-16.4406464494583,-8.09100504150255,
3.55054725653724));
#11416=CARTESIAN_POINT('Ctrl Pts',(-14.2316631334124,-7.69609474266784,
3.44321295131019));
#11417=CARTESIAN_POINT('Ctrl Pts',(-12.647638657407,-9.39608188535426,3.33207180378117));
#11418=CARTESIAN_POINT('Ctrl Pts',(-13.2168727518909,-11.6488717938068,
3.22093065625215));
#11419=CARTESIAN_POINT('Ctrl Pts',(-15.4183110319232,-12.3923496516694,
3.10978950872312));
#11420=CARTESIAN_POINT('Ctrl Pts',(-16.873776480767,-11.2347337715044,3.02083752979319));
#11421=CARTESIAN_POINT('Ctrl Pts',(-17.0532004243018,-10.2759594281538,
2.96893260003959));
#11422=CARTESIAN_POINT('Ctrl Pts',(-17.0519256455684,-10.0010517737669,
2.95407471946232));
#11423=CARTESIAN_POINT('Origin',(-15.,-10.,9.54592528053767));
#11424=CARTESIAN_POINT('',(-17.0555344808246,-9.99819734174245,4.35407471946232));
#11425=CARTESIAN_POINT('',(-17.0526295118996,-10.0014953654714,4.29592528053768));
#11426=CARTESIAN_POINT('',(-17.05475,-9.99999999999991,9.54592528053767));
#11427=CARTESIAN_POINT('Ctrl Pts',(-17.0526295118996,-10.0014953654714,
4.29592528053768));
#11428=CARTESIAN_POINT('Ctrl Pts',(-17.049615748339,-9.55435663972008,4.27173805572604));
#11429=CARTESIAN_POINT('Ctrl Pts',(-16.6860607259798,-8.41788413676447,
4.21050378173805));
#11430=CARTESIAN_POINT('Ctrl Pts',(-14.8104759432562,-7.57876034732949,
4.11222245857374));
#11431=CARTESIAN_POINT('Ctrl Pts',(-12.8629591929671,-8.84614671087597,
4.00108131104471));
#11432=CARTESIAN_POINT('Ctrl Pts',(-12.8716051077936,-11.1697247567595,
3.88994016351569));
#11433=CARTESIAN_POINT('Ctrl Pts',(-14.8284995591272,-12.4225830063246,
3.77879901598667));
#11434=CARTESIAN_POINT('Ctrl Pts',(-16.6925314739129,-11.571923493464,3.680794054994));
#11435=CARTESIAN_POINT('Ctrl Pts',(-17.0496537312629,-10.4406482030388,
3.61983614317767));
#11436=CARTESIAN_POINT('Ctrl Pts',(-17.0525172682208,-9.99855769014068,
3.59592528053768));
#11437=CARTESIAN_POINT('Ctrl Pts',(-17.0555344808246,-9.99819734174245,
4.35407471946232));
#11438=CARTESIAN_POINT('Ctrl Pts',(-17.0567584155299,-9.86475790704786,
4.346830523489));
#11439=CARTESIAN_POINT('Ctrl Pts',(-16.9841133186881,-9.05023169781548,
4.30253927833933));
#11440=CARTESIAN_POINT('Ctrl Pts',(-15.8966028265696,-7.74291684984371,
4.22120098401332));
#11441=CARTESIAN_POINT('Ctrl Pts',(-13.5899069966017,-8.02263845058788,
4.11005983648432));
#11442=CARTESIAN_POINT('Ctrl Pts',(-12.5739545527748,-10.1123586370691,
3.99891868895528));
#11443=CARTESIAN_POINT('Ctrl Pts',(-13.7787081956621,-12.0992301693682,
3.88777754142627));
#11444=CARTESIAN_POINT('Ctrl Pts',(-16.1013840714784,-12.1645493993947,
3.77663639389725));
#11445=CARTESIAN_POINT('Ctrl Pts',(-17.0227508013064,-10.8215719974621,
3.6987354532426));
#11446=CARTESIAN_POINT('Ctrl Pts',(-17.0577395003991,-10.0711616425707,
3.65788156176429));
#11447=CARTESIAN_POINT('Ctrl Pts',(-17.057256555318,-10.001191465967,3.65407471946232));
#11448=CARTESIAN_POINT('Origin',(-15.,-10.,9.54592528053767));
#11449=CARTESIAN_POINT('',(-17.0513922996156,-9.99993062733026,5.05407471946232));
#11450=CARTESIAN_POINT('',(-17.0579125370942,-10.0006073368323,4.99592528053768));
#11451=CARTESIAN_POINT('',(-17.05475,-9.99999999999991,9.54592528053767));
#11452=CARTESIAN_POINT('Ctrl Pts',(-17.0579125370942,-10.0006073368323,
4.99592528053768));
#11453=CARTESIAN_POINT('Ctrl Pts',(-17.0553880289355,-9.3534707240389,4.96068701745074));
#11454=CARTESIAN_POINT('Ctrl Pts',(-16.3773572422904,-8.02142236710827,
4.88840170518746));
#11455=CARTESIAN_POINT('Ctrl Pts',(-14.1088765326179,-7.74074795791574,
4.77906934374786));
#11456=CARTESIAN_POINT('Ctrl Pts',(-12.6185654451633,-9.52346009110162,
4.66792819621883));
#11457=CARTESIAN_POINT('Ctrl Pts',(-13.3081253972587,-11.7423780164876,
4.55678704868982));
#11458=CARTESIAN_POINT('Ctrl Pts',(-15.5463604710685,-12.3663919919164,
4.44564590116079));
#11459=CARTESIAN_POINT('Ctrl Pts',(-16.9062187021531,-11.1599029697348,
4.35869197844342));
#11460=CARTESIAN_POINT('Ctrl Pts',(-17.0542318648098,-10.2392293562288,
4.30878510490238));
#11461=CARTESIAN_POINT('Ctrl Pts',(-17.0526295118996,-10.0014953654714,
4.29592528053768));
#11462=CARTESIAN_POINT('Ctrl Pts',(-17.0513922996156,-9.99993062733025,
5.05407471946232));
#11463=CARTESIAN_POINT('Ctrl Pts',(-17.0514943003483,-9.66120346411399,
5.03577948521371));
#11464=CARTESIAN_POINT('Ctrl Pts',(-16.8117677005034,-8.63670450547305,
4.98043720178875));
#11465=CARTESIAN_POINT('Ctrl Pts',(-15.1953985278237,-7.57922731532253,
4.88804786918744));
#11466=CARTESIAN_POINT('Ctrl Pts',(-13.0721026532078,-8.52299871511589,
4.77690672165843));
#11467=CARTESIAN_POINT('Ctrl Pts',(-12.7135277889139,-10.818758696566,4.6657655741294));
#11468=CARTESIAN_POINT('Ctrl Pts',(-14.4478991890863,-12.3650593375113,
4.55462442660038));
#11469=CARTESIAN_POINT('Ctrl Pts',(-16.5416550956139,-11.7867973751395,
4.45072747504469));
#11470=CARTESIAN_POINT('Ctrl Pts',(-17.0504991744238,-10.5471714305632,
4.38387757266534));
#11471=CARTESIAN_POINT('Ctrl Pts',(-17.0555344808246,-9.99819734174245,
4.35407471946232));
#11472=CARTESIAN_POINT('Origin',(-15.,-10.,9.54592528053767));
#11473=CARTESIAN_POINT('',(-17.0552798090643,-10.0018385066652,5.75407471946232));
#11474=CARTESIAN_POINT('',(-17.0544192972179,-9.99812308974333,5.69592528053768));
#11475=CARTESIAN_POINT('',(-17.05475,-9.99999999999991,9.54592528053767));
#11476=CARTESIAN_POINT('Ctrl Pts',(-17.0544192972179,-9.99812308974333,
5.69592528053768));
#11477=CARTESIAN_POINT('Ctrl Pts',(-17.0559615050427,-9.82764220092783,
5.68668302835179));
#11478=CARTESIAN_POINT('Ctrl Pts',(-16.9585687134996,-8.9755360511576,5.64039372698956));
#11479=CARTESIAN_POINT('Ctrl Pts',(-15.7739249147585,-7.69796588935184,
5.55705737645099));
#11480=CARTESIAN_POINT('Ctrl Pts',(-13.4856097934235,-8.10133122228054,
5.44591622892198));
#11481=CARTESIAN_POINT('Ctrl Pts',(-12.583507594572,-10.2426628903111,5.33477508139295));
#11482=CARTESIAN_POINT('Ctrl Pts',(-13.8933670056466,-12.161870541709,5.22363393386393));
#11483=CARTESIAN_POINT('Ctrl Pts',(-16.2161945081267,-12.1021873709018,
5.11249278633491));
#11484=CARTESIAN_POINT('Ctrl Pts',(-17.0422606408936,-10.7472711004341,
5.03658990189283));
#11485=CARTESIAN_POINT('Ctrl Pts',(-17.0580421205311,-10.0338249701837,
4.99773406662709));
#11486=CARTESIAN_POINT('Ctrl Pts',(-17.0579125370942,-10.0006073368323,
4.99592528053768));
#11487=CARTESIAN_POINT('Ctrl Pts',(-17.0552798090643,-10.0018385066652,
5.75407471946232));
#11488=CARTESIAN_POINT('Ctrl Pts',(-17.05028974167,-9.46110238806226,5.72472844693841));
#11489=CARTESIAN_POINT('Ctrl Pts',(-16.5543371109916,-8.2296373672222,5.65833512523816));
#11490=CARTESIAN_POINT('Ctrl Pts',(-14.4770180600175,-7.62833162617035,
5.55489475436157));
#11491=CARTESIAN_POINT('Ctrl Pts',(-12.7237668001956,-9.15319223134576,
5.44375360683254));
#11492=CARTESIAN_POINT('Ctrl Pts',(-13.0540894216228,-11.4531871843689,
5.33261245930352));
#11493=CARTESIAN_POINT('Ctrl Pts',(-15.1656216518599,-12.4229920439975,
5.22147131177451));
#11494=CARTESIAN_POINT('Ctrl Pts',(-16.8029213911039,-11.380339808568,5.1286253984941));
#11495=CARTESIAN_POINT('Ctrl Pts',(-17.0512877533257,-10.3471111547456,
5.07282653439004));
#11496=CARTESIAN_POINT('Ctrl Pts',(-17.0513922996156,-9.99993062733025,
5.05407471946232));
#11497=CARTESIAN_POINT('Origin',(-15.,-10.,9.54592528053767));
#11498=CARTESIAN_POINT('',(-17.0574372391259,-9.99893002996487,6.45407471946233));
#11499=CARTESIAN_POINT('',(-17.0515170795977,-10.0005308591959,6.39592528053768));
#11500=CARTESIAN_POINT('',(-17.05475,-9.99999999999991,9.54592528053767));
#11501=CARTESIAN_POINT('Ctrl Pts',(-17.0515170795977,-10.0005308591959,
6.39592528053768));
#11502=CARTESIAN_POINT('Ctrl Pts',(-17.0506483964156,-9.62486769760656,
6.3756319900765));
#11503=CARTESIAN_POINT('Ctrl Pts',(-16.771966871107,-8.56220130633378,6.31829165043898));
#11504=CARTESIAN_POINT('Ctrl Pts',(-15.0649324846807,-7.5722223329502,6.22390426162511));
#11505=CARTESIAN_POINT('Ctrl Pts',(-12.995462913005,-8.62881367080874,6.11276311409609));
#11506=CARTESIAN_POINT('Ctrl Pts',(-12.7608673412954,-10.9405348370204,
6.00162196656707));
#11507=CARTESIAN_POINT('Ctrl Pts',(-14.5758852786477,-12.3913275602698,
5.89048081903805));
#11508=CARTESIAN_POINT('Ctrl Pts',(-16.5959048462141,-11.7145751864396,
5.78858192369492));
#11509=CARTESIAN_POINT('Ctrl Pts',(-17.0497796515317,-10.5110052757004,
5.72373007752813));
#11510=CARTESIAN_POINT('Ctrl Pts',(-17.0544192972179,-9.99812308974333,
5.69592528053768));
#11511=CARTESIAN_POINT('Ctrl Pts',(-17.0574372391259,-9.99893002996487,
6.45407471946233));
#11512=CARTESIAN_POINT('Ctrl Pts',(-17.0578271002392,-9.93736608446989,
6.45072445783946));
#11513=CARTESIAN_POINT('Ctrl Pts',(-17.0273958925505,-9.19542143745478,
6.41032714704025));
#11514=CARTESIAN_POINT('Ctrl Pts',(-16.1279126463626,-7.84915537048691,
6.3328827870647));
#11515=CARTESIAN_POINT('Ctrl Pts',(-13.8046094981315,-7.88591323323186,
6.22174163953568));
#11516=CARTESIAN_POINT('Ctrl Pts',(-12.5755192591945,-9.85782298675155,
6.11060049200667));
#11517=CARTESIAN_POINT('Ctrl Pts',(-13.5657029889766,-11.9598757266924,
5.99945934447763));
#11518=CARTESIAN_POINT('Ctrl Pts',(-15.8687854179254,-12.2679358305796,
5.88831819694863));
#11519=CARTESIAN_POINT('Ctrl Pts',(-16.9784808094819,-10.9668273162222,
5.80652332194351));
#11520=CARTESIAN_POINT('Ctrl Pts',(-17.0565892562676,-10.1437334636437,
5.76177549611475));
#11521=CARTESIAN_POINT('Ctrl Pts',(-17.0552798090643,-10.0018385066652,
5.75407471946232));
#11522=CARTESIAN_POINT('Origin',(-15.,-10.,9.54592528053767));
#11523=CARTESIAN_POINT('',(-17.0520596215353,-9.99884120146076,7.15407471946233));
#11524=CARTESIAN_POINT('',(-17.0563656598722,-10.0016028745823,7.09592528053768));
#11525=CARTESIAN_POINT('',(-17.05475,-9.99999999999991,9.54592528053767));
#11526=CARTESIAN_POINT('Ctrl Pts',(-17.0563656598722,-10.0016028745823,
7.09592528053768));
#11527=CARTESIAN_POINT('Ctrl Pts',(-17.0514195939162,-9.42483826837157,
7.0645809518012));
#11528=CARTESIAN_POINT('Ctrl Pts',(-16.4975740702056,-8.15804707939392,
6.99618957388839));
#11529=CARTESIAN_POINT('Ctrl Pts',(-14.350232319384,-7.65989044479182,6.89075114679923));
#11530=CARTESIAN_POINT('Ctrl Pts',(-12.6815213858194,-9.27682682597027,
6.77960999927021));
#11531=CARTESIAN_POINT('Ctrl Pts',(-13.1350541938888,-11.5557312393606,
6.66846885174119));
#11532=CARTESIAN_POINT('Ctrl Pts',(-15.295684618859,-12.4105787711389,6.55732770421217));
#11533=CARTESIAN_POINT('Ctrl Pts',(-16.8405665064385,-11.3056860735596,
6.46647984714433));
#11534=CARTESIAN_POINT('Ctrl Pts',(-17.0522342480855,-10.3106712959811,
6.41267903925284));
#11535=CARTESIAN_POINT('Ctrl Pts',(-17.0515170795977,-10.0005308591959,
6.39592528053768));
#11536=CARTESIAN_POINT('Ctrl Pts',(-17.0520596215353,-9.99884120146076,
7.15407471946233));
#11537=CARTESIAN_POINT('Ctrl Pts',(-17.053436293058,-9.73242147652985,7.13967341956416));
#11538=CARTESIAN_POINT('Ctrl Pts',(-16.8814296172514,-8.78234594443343,
7.08822507048967));
#11539=CARTESIAN_POINT('Ctrl Pts',(-15.4476835001917,-7.61298704116733,
6.99972967223882));
#11540=CARTESIAN_POINT('Ctrl Pts',(-13.2372839439424,-8.32932353917012,
6.88858852470981));
#11541=CARTESIAN_POINT('Ctrl Pts',(-12.64038931445,-10.5749548961775,6.77744737718078));
#11542=CARTESIAN_POINT('Ctrl Pts',(-14.2033970972384,-12.2942830560246,
6.66630622965177));
#11543=CARTESIAN_POINT('Ctrl Pts',(-16.4264834956963,-11.9249992699025,
6.55851534374561));
#11544=CARTESIAN_POINT('Ctrl Pts',(-17.0535160327875,-10.618137550398,6.4877715070158));
#11545=CARTESIAN_POINT('Ctrl Pts',(-17.0574372391259,-9.99893002996487,
6.45407471946233));
#11546=CARTESIAN_POINT('Origin',(-15.,-10.,9.54592528053767));
#11547=CARTESIAN_POINT('',(-17.0526884867324,-10.0024695060038,7.85407471946233));
#11548=CARTESIAN_POINT('',(-17.0565470023424,-9.99851185632501,7.79592528053768));
#11549=CARTESIAN_POINT('',(-17.05475,-9.99999999999991,9.54592528053767));
#11550=CARTESIAN_POINT('',(-15.5301702171886,-11.9851743256717,8.));
#11551=CARTESIAN_POINT('Ctrl Pts',(-15.5301702171886,-11.9851743256717,
8.));
#11552=CARTESIAN_POINT('Ctrl Pts',(-16.1903072548812,-11.8088749487748,
7.96295295082366));
#11553=CARTESIAN_POINT('Ctrl Pts',(-16.9250043904129,-11.1129876322537,
7.91431119064444));
#11554=CARTESIAN_POINT('Ctrl Pts',(-17.0543121182783,-10.216714563805,7.86566943046521));
#11555=CARTESIAN_POINT('Ctrl Pts',(-17.0526884867324,-10.0024695060038,
7.85407471946233));
#11556=CARTESIAN_POINT('',(-14.4687304269164,-11.988749893056,8.));
#11557=CARTESIAN_POINT('Origin',(-15.,-10.,8.));
#11558=CARTESIAN_POINT('Ctrl Pts',(-14.4687300448211,-11.9887511357905,
8.));
#11559=CARTESIAN_POINT('Ctrl Pts',(-15.1134147663027,-12.1601152915704,
7.96367382485347));
#11560=CARTESIAN_POINT('Ctrl Pts',(-16.4930658496611,-11.8405006708346,
7.89564891836603));
#11561=CARTESIAN_POINT('Ctrl Pts',(-17.0516776590012,-10.5815167296829,
7.82762401187859));
#11562=CARTESIAN_POINT('Ctrl Pts',(-17.0565470023424,-9.99851185632501,
7.79592528053768));
#11563=CARTESIAN_POINT('Origin',(12.9142135623731,11.9142135623731,26.));
#11564=CARTESIAN_POINT('',(18.,6.82842712474619,28.));
#11565=CARTESIAN_POINT('',(12.8284271247462,12.,28.));
#11566=CARTESIAN_POINT('',(12.9142135623731,11.9142135623731,28.));
#11567=CARTESIAN_POINT('',(12.,10.,26.));
#11568=CARTESIAN_POINT('Origin',(12.8284271247462,12.,26.));
#11569=CARTESIAN_POINT('',(16.,6.,26.));
#11570=CARTESIAN_POINT('',(11.5,10.5,26.));
#11571=CARTESIAN_POINT('Origin',(18.,6.82842712474619,26.));
#11572=CARTESIAN_POINT('Origin',(-6.,12.,26.));
#11573=CARTESIAN_POINT('',(-12.8284271247462,12.,28.));
#11574=CARTESIAN_POINT('',(-6.,12.,28.));
#11575=CARTESIAN_POINT('',(-12.,10.,26.));
#11576=CARTESIAN_POINT('Origin',(-12.8284271247462,12.,26.));
#11577=CARTESIAN_POINT('',(-6.,10.,26.));
#11578=CARTESIAN_POINT('Origin',(-14.9142135623731,9.9142135623731,26.));
#11579=CARTESIAN_POINT('',(-18.,6.82842712474619,28.));
#11580=CARTESIAN_POINT('',(-14.9142135623731,9.9142135623731,28.));
#11581=CARTESIAN_POINT('',(-16.,6.,26.));
#11582=CARTESIAN_POINT('Origin',(-18.,6.82842712474619,26.));
#11583=CARTESIAN_POINT('',(-13.5,8.5,26.));
#11584=CARTESIAN_POINT('Origin',(-18.,-5.,26.));
#11585=CARTESIAN_POINT('',(-18.,-12.,28.));
#11586=CARTESIAN_POINT('',(-18.,-5.,28.));
#11587=CARTESIAN_POINT('',(-16.,-10.,26.));
#11588=CARTESIAN_POINT('Origin',(-18.,-12.,26.));
#11589=CARTESIAN_POINT('',(-16.,-5.,26.));
#11590=CARTESIAN_POINT('Origin',(8.,-12.,26.));
#11591=CARTESIAN_POINT('',(16.,-10.,26.));
#11592=CARTESIAN_POINT('',(8.,-10.,26.));
#11593=CARTESIAN_POINT('',(18.,-12.,28.));
#11594=CARTESIAN_POINT('',(8.,-12.,28.));
#11595=CARTESIAN_POINT('Origin',(18.,-12.,26.));
#11596=CARTESIAN_POINT('Origin',(18.,3.,26.));
#11597=CARTESIAN_POINT('',(16.,3.,26.));
#11598=CARTESIAN_POINT('',(18.,3.,28.));
#11599=CARTESIAN_POINT('Origin',(16.,-10.,0.));
#11600=CARTESIAN_POINT('',(16.,-10.,8.));
#11601=CARTESIAN_POINT('',(16.,-10.,0.));
#11602=CARTESIAN_POINT('',(13.1979999955782,-10.0000000206464,8.));
#11603=CARTESIAN_POINT('',(8.,-10.,8.));
#11604=CARTESIAN_POINT('',(-13.198,-10.,8.));
#11605=CARTESIAN_POINT('',(8.,-10.,8.));
#11606=CARTESIAN_POINT('',(-16.,-10.,8.));
#11607=CARTESIAN_POINT('',(8.,-10.,8.));
#11608=CARTESIAN_POINT('',(-16.,-10.,0.));
#11609=CARTESIAN_POINT('Origin',(16.,6.,0.));
#11610=CARTESIAN_POINT('',(16.,6.,8.));
#11611=CARTESIAN_POINT('',(16.,6.,0.));
#11612=CARTESIAN_POINT('',(16.,3.,8.));
#11613=CARTESIAN_POINT('',(16.,3.,8.));
#11614=CARTESIAN_POINT('Origin',(12.,10.,0.));
#11615=CARTESIAN_POINT('',(12.,10.,8.));
#11616=CARTESIAN_POINT('',(12.,10.,0.));
#11617=CARTESIAN_POINT('',(11.5,10.5,8.));
#11618=CARTESIAN_POINT('Origin',(0.,0.,28.));
#11619=CARTESIAN_POINT('',(32.,-3.77491721763538,28.));
#11620=CARTESIAN_POINT('',(32.,-18.,28.));
#11621=CARTESIAN_POINT('',(32.,-10.,28.));
#11622=CARTESIAN_POINT('',(32.,3.77491721763538,28.));
#11623=CARTESIAN_POINT('Origin',(28.,0.,28.));
#11624=CARTESIAN_POINT('',(32.,18.,28.));
#11625=CARTESIAN_POINT('',(32.,-10.,28.));
#11626=CARTESIAN_POINT('',(-32.,18.,28.));
#11627=CARTESIAN_POINT('',(17.,18.,28.));
#11628=CARTESIAN_POINT('',(-32.,3.77491721763538,28.));
#11629=CARTESIAN_POINT('',(-32.,10.,28.));
#11630=CARTESIAN_POINT('',(-22.5,-6.73555739531045E-16,28.));
#11631=CARTESIAN_POINT('Origin',(-28.,0.,28.));
#11632=CARTESIAN_POINT('',(-32.,-3.77491721763538,28.));
#11633=CARTESIAN_POINT('Origin',(-28.,0.,28.));
#11634=CARTESIAN_POINT('',(-32.,-18.,28.));
#11635=CARTESIAN_POINT('',(-32.,10.,28.));
#11636=CARTESIAN_POINT('',(-17.,-18.,28.));
#11637=CARTESIAN_POINT('Origin',(32.,-10.,26.));
#11638=CARTESIAN_POINT('',(32.75,-6.37798309992857E-16,27.8540496217739));
#11639=CARTESIAN_POINT('Ctrl Pts',(32.,3.77491721763538,28.));
#11640=CARTESIAN_POINT('Ctrl Pts',(32.0019525144519,3.77000349735399,28.));
#11641=CARTESIAN_POINT('Ctrl Pts',(32.0039017377963,3.76508846538185,27.9999971407691));
#11642=CARTESIAN_POINT('Ctrl Pts',(32.2437689219487,3.15906880248546,27.9992958069976));
#11643=CARTESIAN_POINT('Ctrl Pts',(32.4320766813924,2.53932916982673,27.9572986150603));
#11644=CARTESIAN_POINT('Ctrl Pts',(32.6335924011263,1.53220364744403,27.8985426691076));
#11645=CARTESIAN_POINT('Ctrl Pts',(32.6866197302491,1.16003166445502,27.8787386406688));
#11646=CARTESIAN_POINT('Ctrl Pts',(32.7391880669654,0.522990467484402,27.8585298486776));
#11647=CARTESIAN_POINT('Ctrl Pts',(32.75,0.262060967255928,27.8540496217739));
#11648=CARTESIAN_POINT('Ctrl Pts',(32.75,-6.93889390390723E-16,27.8540496217739));
#11649=CARTESIAN_POINT('Ctrl Pts',(32.75,-6.93889390390723E-16,27.8540496217739));
#11650=CARTESIAN_POINT('Ctrl Pts',(32.75,-0.262060967255973,27.8540496217739));
#11651=CARTESIAN_POINT('Ctrl Pts',(32.7391880669654,-0.522990467484491,
27.8585298486776));
#11652=CARTESIAN_POINT('Ctrl Pts',(32.6866197302491,-1.16003166445499,27.8787386406688));
#11653=CARTESIAN_POINT('Ctrl Pts',(32.6335924011263,-1.53220364744395,27.8985426691076));
#11654=CARTESIAN_POINT('Ctrl Pts',(32.4320766813953,-2.53932916981226,27.9572986150594));
#11655=CARTESIAN_POINT('Ctrl Pts',(32.2437689219548,-3.15906880247018,27.9992958069976));
#11656=CARTESIAN_POINT('Ctrl Pts',(32.0039017377962,-3.76508846538219,27.9999971407691));
#11657=CARTESIAN_POINT('Ctrl Pts',(32.001952514452,-3.77000349735365,28.));
#11658=CARTESIAN_POINT('Ctrl Pts',(32.,-3.77491721763538,28.));
#11659=CARTESIAN_POINT('',(34.,-20.,26.));
#11660=CARTESIAN_POINT('Origin',(32.,-18.,26.));
#11661=CARTESIAN_POINT('',(34.,20.,26.));
#11662=CARTESIAN_POINT('',(34.,-10.,26.));
#11663=CARTESIAN_POINT('Origin',(32.,18.,26.));
#11664=CARTESIAN_POINT('Origin',(-17.,-18.,26.));
#11665=CARTESIAN_POINT('',(-34.,-20.,26.));
#11666=CARTESIAN_POINT('Origin',(-32.,-18.,26.));
#11667=CARTESIAN_POINT('',(-17.,-20.,26.));
#11668=CARTESIAN_POINT('Origin',(-32.,10.,26.));
#11669=CARTESIAN_POINT('Ctrl Pts',(-32.,-3.77491721763538,28.));
#11670=CARTESIAN_POINT('Ctrl Pts',(-32.0019525144519,-3.77000349735395,
28.));
#11671=CARTESIAN_POINT('Ctrl Pts',(-32.0039017377963,-3.7650884653819,27.9999971407691));
#11672=CARTESIAN_POINT('Ctrl Pts',(-32.2437689219487,-3.15906880248546,
27.9992958069976));
#11673=CARTESIAN_POINT('Ctrl Pts',(-32.4320766813924,-2.53932916982673,
27.9572986150603));
#11674=CARTESIAN_POINT('Ctrl Pts',(-32.6335924011263,-1.53220364744392,
27.8985426691076));
#11675=CARTESIAN_POINT('Ctrl Pts',(-32.6866197302491,-1.16003166445497,
27.8787386406688));
#11676=CARTESIAN_POINT('Ctrl Pts',(-32.7391880669654,-0.522990467484492,
27.8585298486776));
#11677=CARTESIAN_POINT('Ctrl Pts',(-32.75,-0.262060967255973,27.8540496217739));
#11678=CARTESIAN_POINT('Ctrl Pts',(-32.75,0.262060967255972,27.8540496217739));
#11679=CARTESIAN_POINT('Ctrl Pts',(-32.7391880669654,0.52299046748449,27.8585298486776));
#11680=CARTESIAN_POINT('Ctrl Pts',(-32.6866197302491,1.16003166445499,27.8787386406688));
#11681=CARTESIAN_POINT('Ctrl Pts',(-32.6335924011263,1.53220364744395,27.8985426691076));
#11682=CARTESIAN_POINT('Ctrl Pts',(-32.4320766813924,2.53932916982672,27.9572986150603));
#11683=CARTESIAN_POINT('Ctrl Pts',(-32.2437689219487,3.15906880248545,27.9992958069976));
#11684=CARTESIAN_POINT('Ctrl Pts',(-32.0039017377963,3.7650884653819,27.9999971407691));
#11685=CARTESIAN_POINT('Ctrl Pts',(-32.0019525144519,3.77000349735395,28.));
#11686=CARTESIAN_POINT('Ctrl Pts',(-32.,3.77491721763538,28.));
#11687=CARTESIAN_POINT('',(-34.,20.,26.));
#11688=CARTESIAN_POINT('Origin',(-32.,18.,26.));
#11689=CARTESIAN_POINT('',(-34.,10.,26.));
#11690=CARTESIAN_POINT('Origin',(17.,18.,26.));
#11691=CARTESIAN_POINT('',(17.,20.,26.));
#11692=CARTESIAN_POINT('Origin',(34.,20.,24.));
#11693=CARTESIAN_POINT('',(34.,20.,24.));
#11694=CARTESIAN_POINT('',(34.,20.,24.));
#11695=CARTESIAN_POINT('',(-34.,20.,24.));
#11696=CARTESIAN_POINT('',(34.,20.,24.));
#11697=CARTESIAN_POINT('',(-34.,20.,24.));
#11698=CARTESIAN_POINT('Origin',(34.,-20.,24.));
#11699=CARTESIAN_POINT('',(34.,-20.,24.));
#11700=CARTESIAN_POINT('',(34.,-20.,24.));
#11701=CARTESIAN_POINT('',(34.,-20.,24.));
#11702=CARTESIAN_POINT('Origin',(28.,0.,26.));
#11703=CARTESIAN_POINT('',(31.5,-6.16297582203915E-32,26.));
#11704=CARTESIAN_POINT('Origin',(33.5,-6.73555739531044E-16,26.));
#11705=CARTESIAN_POINT('',(24.5,4.28626379701574E-16,26.));
#11706=CARTESIAN_POINT('Origin',(28.,0.,26.));
#11707=CARTESIAN_POINT('Origin',(28.,0.,26.));
#11708=CARTESIAN_POINT('Origin',(-28.,0.,26.));
#11709=CARTESIAN_POINT('',(-24.5,-6.16297582203915E-32,26.));
#11710=CARTESIAN_POINT('Origin',(-22.5,-6.73555739531044E-16,26.));
#11711=CARTESIAN_POINT('',(-31.5,4.28626379701574E-16,26.));
#11712=CARTESIAN_POINT('Origin',(-28.,0.,26.));
#11713=CARTESIAN_POINT('Origin',(-28.,0.,26.));
#11714=CARTESIAN_POINT('Origin',(28.,0.,26.));
#11715=CARTESIAN_POINT('',(24.5,4.28626379701574E-16,24.));
#11716=CARTESIAN_POINT('',(24.5,4.28626379701574E-16,26.));
#11717=CARTESIAN_POINT('Origin',(28.,0.,24.));
#11718=CARTESIAN_POINT('Origin',(-28.,0.,26.));
#11719=CARTESIAN_POINT('',(-31.5,4.28626379701574E-16,24.));
#11720=CARTESIAN_POINT('',(-31.5,4.28626379701574E-16,26.));
#11721=CARTESIAN_POINT('Origin',(-28.,0.,24.));
#11722=CARTESIAN_POINT('Origin',(-15.,-10.,9.54592528053767));
#11723=CARTESIAN_POINT('Ctrl Pts',(-17.0565470023424,-9.99851185632501,
7.79592528053768));
#11724=CARTESIAN_POINT('Ctrl Pts',(-17.0573685745232,-9.90014528989089,
7.79057696270225));
#11725=CARTESIAN_POINT('Ctrl Pts',(-17.0062396084505,-9.12123442332477,
7.74818159569048));
#11726=CARTESIAN_POINT('Ctrl Pts',(-16.0106088364074,-7.79139167661744,
7.66873917950237));
#11727=CARTESIAN_POINT('Ctrl Pts',(-13.6926511338527,-7.95337102943111,
7.55759803197335));
#11728=CARTESIAN_POINT('Ctrl Pts',(-12.5713805503198,-9.98835294159719,
7.44645688444433));
#11729=CARTESIAN_POINT('Ctrl Pts',(-13.6731764957754,-12.0342028340593,
7.3353157369153));
#11730=CARTESIAN_POINT('Ctrl Pts',(-15.989492000612,-12.2179172171411,7.22417458938629));
#11731=CARTESIAN_POINT('Ctrl Pts',(-17.0022526535647,-10.8922265068485,
7.14437777059375));
#11732=CARTESIAN_POINT('Ctrl Pts',(-17.0572655365823,-10.1065381991343,
7.10162800097754));
#11733=CARTESIAN_POINT('Ctrl Pts',(-17.0563656598722,-10.0016028745823,
7.09592528053768));
#11734=CARTESIAN_POINT('Ctrl Pts',(-17.0526884867324,-10.0024695060038,
7.85407471946233));
#11735=CARTESIAN_POINT('Ctrl Pts',(-17.0491243427736,-9.53216561815421,
7.82862238128887));
#11736=CARTESIAN_POINT('Ctrl Pts',(-16.6564412157395,-8.37020235436293,
7.76612299393908));
#11737=CARTESIAN_POINT('Ctrl Pts',(-14.727662200004,-7.58731060863186,7.66657655741293));
#11738=CARTESIAN_POINT('Ctrl Pts',(-12.8251332301876,-8.91924943693317,
7.55543540988393));
#11739=CARTESIAN_POINT('Ctrl Pts',(-12.9125601407559,-11.2417229038903,
7.4442942623549));
#11740=CARTESIAN_POINT('Ctrl Pts',(-14.9111754350777,-12.4269243298781,
7.33315311482589));
#11741=CARTESIAN_POINT('Ctrl Pts',(-16.721395498903,-11.5251875586803,7.23641326719502));
#11742=CARTESIAN_POINT('Ctrl Pts',(-17.0498948337479,-10.417780764987,7.1767204687405));
#11743=CARTESIAN_POINT('Ctrl Pts',(-17.0520596215353,-9.99884120146076,
7.15407471946233));
#11744=CARTESIAN_POINT('Ctrl Pts',(-13.7309291201476,-8.92064134695149,
8.));
#11745=CARTESIAN_POINT('Ctrl Pts',(-13.3720061708544,-9.34264997380806,
7.96295295082366));
#11746=CARTESIAN_POINT('Ctrl Pts',(-13.1145386540675,-10.5656659613133,
7.88885885247098));
#11747=CARTESIAN_POINT('Ctrl Pts',(-14.4551162761764,-11.893574716725,7.77771770494197));
#11748=CARTESIAN_POINT('Ctrl Pts',(-16.2942887603119,-11.4833631126878,
7.66657655741294));
#11749=CARTESIAN_POINT('Ctrl Pts',(-16.9487772336236,-9.71772814539447,
7.55543540988392));
#11750=CARTESIAN_POINT('Ctrl Pts',(-15.8194059235697,-8.20925101995117,
7.4442942623549));
#11751=CARTESIAN_POINT('Ctrl Pts',(-13.9399960038928,-8.34058456504792,
7.33315311482588));
#11752=CARTESIAN_POINT('Ctrl Pts',(-13.0308650672018,-9.9905565157323,7.22201196729686));
#11753=CARTESIAN_POINT('Ctrl Pts',(-13.9242058848823,-11.6493402708567,
7.11087081976784));
#11754=CARTESIAN_POINT('Ctrl Pts',(-15.8022843036961,-11.798296670523,6.99972967223882));
#11755=CARTESIAN_POINT('Ctrl Pts',(-16.9459843182726,-10.3012080146147,
6.88858852470981));
#11756=CARTESIAN_POINT('Ctrl Pts',(-16.3084067449585,-8.52838242895221,
6.77744737718078));
#11757=CARTESIAN_POINT('Ctrl Pts',(-14.4731656133806,-8.10262926439867,
6.66630622965177));
#11758=CARTESIAN_POINT('Ctrl Pts',(-13.1201677229713,-9.41364812851512,
6.55516508212274));
#11759=CARTESIAN_POINT('Ctrl Pts',(-13.4878940440534,-11.2613934759824,
6.44402393459372));
#11760=CARTESIAN_POINT('Ctrl Pts',(-15.2397423409267,-11.9545074742511,
6.33288278706471));
#11761=CARTESIAN_POINT('Ctrl Pts',(-16.7721399948386,-10.8585434454103,
6.22174163953568));
#11762=CARTESIAN_POINT('Ctrl Pts',(-16.6823907514308,-8.97670225553072,
6.11060049200667));
#11763=CARTESIAN_POINT('Ctrl Pts',(-15.0526475335092,-8.03154758812267,
5.99945934447764));
#11764=CARTESIAN_POINT('Ctrl Pts',(-13.3747128424705,-8.888236318563,5.88831819694863));
#11765=CARTESIAN_POINT('Ctrl Pts',(-13.1845017596292,-10.7625896281669,
5.7771770494196));
#11766=CARTESIAN_POINT('Ctrl Pts',(-14.6561259881869,-11.938898510967,5.66603590189058));
#11767=CARTESIAN_POINT('Ctrl Pts',(-16.4425188921508,-11.3404163686345,
5.55489475436156));
#11768=CARTESIAN_POINT('Ctrl Pts',(-16.908487033224,-9.51497006870877,5.44375360683254));
#11769=CARTESIAN_POINT('Ctrl Pts',(-15.6275015977553,-8.13350099606285,
5.33261245930353));
#11770=CARTESIAN_POINT('Ctrl Pts',(-13.7721260084407,-8.46055131588728,
5.22147131177451));
#11771=CARTESIAN_POINT('Ctrl Pts',(-13.0406977260285,-10.1967520989212,
5.11033016424549));
#11772=CARTESIAN_POINT('Ctrl Pts',(-14.1027372825927,-11.7528537887758,
4.99918901671646));
#11773=CARTESIAN_POINT('Ctrl Pts',(-15.9860956566683,-11.7044624211814,
4.88804786918745));
#11774=CARTESIAN_POINT('Ctrl Pts',(-16.9668210527183,-10.0958735403876,
4.77690672165842));
#11775=CARTESIAN_POINT('Ctrl Pts',(-16.1471962169778,-8.39952581124097,
4.6657655741294));
#11776=CARTESIAN_POINT('Ctrl Pts',(-14.2774733195481,-8.16818887839767,
4.55462442660039));
#11777=CARTESIAN_POINT('Ctrl Pts',(-13.069122779726,-9.61361942415149,4.44348327907136));
#11778=CARTESIAN_POINT('Ctrl Pts',(-13.628220908545,-11.4127274731565,4.33234213154235));
#11779=CARTESIAN_POINT('Ctrl Pts',(-15.4429913832827,-11.9186806465666,
4.22120098401332));
#11780=CARTESIAN_POINT('Ctrl Pts',(-16.8522650597871,-10.6683494127027,
4.11005983648431));
#11781=CARTESIAN_POINT('Ctrl Pts',(-16.5660485313643,-8.80623755018859,
3.99891868895528));
#11782=CARTESIAN_POINT('Ctrl Pts',(-14.8463330923299,-8.03684863786395,
3.88777754142627));
#11783=CARTESIAN_POINT('Ctrl Pts',(-13.2672782652309,-9.06445086765756,
3.77663639389725));
#11784=CARTESIAN_POINT('Ctrl Pts',(-13.2742884095798,-10.9484177855025,
3.66549524636822));
#11785=CARTESIAN_POINT('Ctrl Pts',(-14.8609467163918,-11.9642405589667,
3.55435409883921));
#11786=CARTESIAN_POINT('Ctrl Pts',(-16.5748889014339,-11.182075182594,3.44321295131019));
#11787=CARTESIAN_POINT('Ctrl Pts',(-16.8472400506147,-9.31788491838175,
3.33207180378117));
#11788=CARTESIAN_POINT('Ctrl Pts',(-15.4287006895954,-8.07807583189886,
3.22093065625215));
#11789=CARTESIAN_POINT('Ctrl Pts',(-13.6177456663529,-8.59752014408551,
3.10978950872313));
#11790=CARTESIAN_POINT('Ctrl Pts',(-13.0720516115789,-10.4007390681565,
2.99864836119411));
#11791=CARTESIAN_POINT('Ctrl Pts',(-14.2911252885726,-11.8371372928603,
2.88750721366509));
#11792=CARTESIAN_POINT('Ctrl Pts',(-16.1590748504492,-11.5918926722399,
2.77636606613607));
#11793=CARTESIAN_POINT('Ctrl Pts',(-16.9660531192297,-9.88949243651641,
2.66522491860705));
#11794=CARTESIAN_POINT('Ctrl Pts',(-15.9733840920941,-8.28824645482409,
2.55408377107803));
#11795=CARTESIAN_POINT('Ctrl Pts',(-14.0897177507374,-8.25387199393599,
2.44294262354901));
#11796=CARTESIAN_POINT('Ctrl Pts',(-13.0392877913138,-9.8178340730497,2.33180147601999));
#11797=CARTESIAN_POINT('Ctrl Pts',(-13.7836162699446,-11.5485436438058,
2.22066032849097));
#11798=CARTESIAN_POINT('Ctrl Pts',(-15.6413743232439,-11.8617775778309,
2.10951918096195));
#11799=CARTESIAN_POINT('Ctrl Pts',(-16.9120436804446,-10.4708139397355,
1.99837803343293));
#11800=CARTESIAN_POINT('Ctrl Pts',(-16.4325038426079,-8.64888580471299,
1.88723688590391));
#11801=CARTESIAN_POINT('Ctrl Pts',(-14.6417066305057,-8.06371424578222,
1.77609573837489));
#11802=CARTESIAN_POINT('Ctrl Pts',(-13.1788769878056,-9.25094199904707,
1.66495459084587));
#11803=CARTESIAN_POINT('Ctrl Pts',(-13.3830313811546,-11.1238280538555,
1.55381344331685));
#11804=CARTESIAN_POINT('Ctrl Pts',(-15.0672948613758,-11.9680059091803,
1.44267229578783));
#11805=CARTESIAN_POINT('Ctrl Pts',(-16.6899593997283,-11.0107497962058,
1.33153114825881));
#11806=CARTESIAN_POINT('Ctrl Pts',(-16.7657016971608,-9.12829166368782,
1.22039000072979));
#11807=CARTESIAN_POINT('Ctrl Pts',(-15.2251908964839,-8.04376401234878,
1.10924885320077));
#11808=CARTESIAN_POINT('Ctrl Pts',(-13.4785484246367,-8.74989136892269,
0.998107705671749));
#11809=CARTESIAN_POINT('Ctrl Pts',(-13.1245841771335,-10.6003305142777,
0.88696655814273));
#11810=CARTESIAN_POINT('Ctrl Pts',(-14.4872983188498,-11.9012280255974,
0.775825410613709));
#11811=CARTESIAN_POINT('Ctrl Pts',(-16.3193253350176,-11.4618607893957,
0.66468426308469));
#11812=CARTESIAN_POINT('Ctrl Pts',(-16.9436824216117,-9.68427827620017,
0.55354311555567));
#11813=CARTESIAN_POINT('Ctrl Pts',(-15.788892098895,-8.19586106027792,0.44240196802665));
#11814=CARTESIAN_POINT('Ctrl Pts',(-13.9119372726392,-8.3585593283779,0.331260820497631));
#11815=CARTESIAN_POINT('Ctrl Pts',(-13.031037036911,-10.0243917235043,0.22011967296861));
#11816=CARTESIAN_POINT('Ctrl Pts',(-13.9522832423509,-11.6666850676998,
0.10897852543959));
#11817=CARTESIAN_POINT('Ctrl Pts',(-15.8328835456553,-11.7857291171073,
-0.00216262208942913));
#11818=CARTESIAN_POINT('Ctrl Pts',(-16.9505137600752,-10.2654025971077,
-0.113303769618449));
#11819=CARTESIAN_POINT('Ctrl Pts',(-16.5058833578897,-9.0973437658213,-0.187397867971129));
#11820=CARTESIAN_POINT('Ctrl Pts',(-16.0856682637066,-8.73632265938642,
-0.224444917147469));
#11821=CARTESIAN_POINT('Ctrl Pts',(-13.6322193753412,-8.83668763019027,
8.07481497238249));
#11822=CARTESIAN_POINT('Ctrl Pts',(-13.2453789997699,-9.29152055750512,
8.03776792320615));
#11823=CARTESIAN_POINT('Ctrl Pts',(-12.9678853731089,-10.6096640890565,
7.96367382485346));
#11824=CARTESIAN_POINT('Ctrl Pts',(-14.4127346139843,-12.0408590646896,
7.85253267732446));
#11825=CARTESIAN_POINT('Ctrl Pts',(-16.394959979914,-11.5987407457524,7.74139152979542));
#11826=CARTESIAN_POINT('Ctrl Pts',(-17.1003552947622,-9.69577272653137,
7.63025038226641));
#11827=CARTESIAN_POINT('Ctrl Pts',(-15.8831402278489,-8.06996457217325,
7.51910923473739));
#11828=CARTESIAN_POINT('Ctrl Pts',(-13.8575477138794,-8.21151338650899,
7.40796808720837));
#11829=CARTESIAN_POINT('Ctrl Pts',(-12.8777035615744,-9.98982199102059,
7.29682693967935));
#11830=CARTESIAN_POINT('Ctrl Pts',(-13.8405294218466,-11.7776277919242,
7.18568579215033));
#11831=CARTESIAN_POINT('Ctrl Pts',(-15.8646868693347,-11.9381701860624,
7.0745446446213));
#11832=CARTESIAN_POINT('Ctrl Pts',(-17.0973451433484,-10.3246363090688,
6.96340349709229));
#11833=CARTESIAN_POINT('Ctrl Pts',(-16.4101760771119,-8.41391837718253,
6.85226234956327));
#11834=CARTESIAN_POINT('Ctrl Pts',(-14.4321878487151,-7.95504965786306,
6.74112120203425));
#11835=CARTESIAN_POINT('Ctrl Pts',(-12.973952277254,-9.36804102766683,6.62998005450523));
#11836=CARTESIAN_POINT('Ctrl Pts',(-13.3702807606652,-11.3595060637751,
6.51883890697621));
#11837=CARTESIAN_POINT('Ctrl Pts',(-15.2583897669041,-12.1065312398804,
6.40769775944719));
#11838=CARTESIAN_POINT('Ctrl Pts',(-16.9099790150454,-10.9253219096766,
6.29655661191817));
#11839=CARTESIAN_POINT('Ctrl Pts',(-16.8132489756442,-8.89710901860346,
6.18541546438915));
#11840=CARTESIAN_POINT('Ctrl Pts',(-15.0567425172331,-7.87843916973185,
6.07427431686013));
#11841=CARTESIAN_POINT('Ctrl Pts',(-13.2482961993154,-8.80176210264491,
5.96313316933111));
#11842=CARTESIAN_POINT('Ctrl Pts',(-13.0432902868512,-10.8219046977847,
5.8519920218021));
#11843=CARTESIAN_POINT('Ctrl Pts',(-14.6293790850072,-12.0897081940679,
5.74085087427307));
#11844=CARTESIAN_POINT('Ctrl Pts',(-16.5547196163051,-11.4446754449263,
5.62970972674406));
#11845=CARTESIAN_POINT('Ctrl Pts',(-17.056931277755,-9.47724390108383,5.51856857921503));
#11846=CARTESIAN_POINT('Ctrl Pts',(-15.6763093700897,-7.98832262715918,
5.40742743168601));
#11847=CARTESIAN_POINT('Ctrl Pts',(-13.676620603435,-8.34081128468504,5.296286284157));
#11848=CARTESIAN_POINT('Ctrl Pts',(-12.888301015543,-10.2120556960512,5.18514513662797));
#11849=CARTESIAN_POINT('Ctrl Pts',(-14.0329471902773,-11.8891927064202,
5.07400398909895));
#11850=CARTESIAN_POINT('Ctrl Pts',(-16.0627952738211,-11.8370374044215,
4.96286284156994));
#11851=CARTESIAN_POINT('Ctrl Pts',(-17.119802582179,-10.1033306910129,4.85172169404091));
#11852=CARTESIAN_POINT('Ctrl Pts',(-16.236426414927,-8.27503914839981,4.7405805465119));
#11853=CARTESIAN_POINT('Ctrl Pts',(-14.2212743905714,-8.02570857157036,
4.62943939898287));
#11854=CARTESIAN_POINT('Ctrl Pts',(-12.9189370015384,-9.58356631313487,
4.51829825145385));
#11855=CARTESIAN_POINT('Ctrl Pts',(-13.5215224047829,-11.5226109876002,
4.40715710392484));
#11856=CARTESIAN_POINT('Ctrl Pts',(-15.477447745878,-12.0679177616832,4.29601595639581));
#11857=CARTESIAN_POINT('Ctrl Pts',(-16.9963362966803,-10.7203343735246,
4.18487480886679));
#11858=CARTESIAN_POINT('Ctrl Pts',(-16.6878575282767,-8.71338537884723,
4.07373366133777));
#11859=CARTESIAN_POINT('Ctrl Pts',(-14.8343807093053,-7.88415254101912,
3.96259251380876));
#11860=CARTESIAN_POINT('Ctrl Pts',(-13.1325052411429,-8.99168281539703,
3.85145136627973));
#11861=CARTESIAN_POINT('Ctrl Pts',(-13.1400606423177,-11.0221867759215,
3.74031021875072));
#11862=CARTESIAN_POINT('Ctrl Pts',(-14.8501309973036,-12.1170213747526,
3.62916907122169));
#11863=CARTESIAN_POINT('Ctrl Pts',(-16.6973855121647,-11.2740183052897,
3.51802792369268));
#11864=CARTESIAN_POINT('Ctrl Pts',(-16.9909204367044,-9.26482924851799,
3.40688677616366));
#11865=CARTESIAN_POINT('Ctrl Pts',(-15.4620455061381,-7.92858643206906,
3.29574562863463));
#11866=CARTESIAN_POINT('Ctrl Pts',(-13.5102323866,-8.48843370071082,3.18460448110562));
#11867=CARTESIAN_POINT('Ctrl Pts',(-12.922093641191,-10.4319089986779,3.07346333357659));
#11868=CARTESIAN_POINT('Ctrl Pts',(-14.2359882249336,-11.9800318752131,
2.96232218604758));
#11869=CARTESIAN_POINT('Ctrl Pts',(-16.2492289817241,-11.7157118551798,
2.85118103851855));
#11870=CARTESIAN_POINT('Ctrl Pts',(-17.1189749179693,-9.88089703529509,
2.74003989098954));
#11871=CARTESIAN_POINT('Ctrl Pts',(-16.0490949896134,-8.15510435984867,
2.62889874346051));
#11872=CARTESIAN_POINT('Ctrl Pts',(-14.0189149847508,-8.11805621515299,
2.5177575959315));
#11873=CARTESIAN_POINT('Ctrl Pts',(-12.8867814145378,-9.80366500460193,
2.40661644840247));
#11874=CARTESIAN_POINT('Ctrl Pts',(-13.6890045902609,-11.6689910910907,
2.29547530087346));
#11875=CARTESIAN_POINT('Ctrl Pts',(-15.6912611315994,-12.0065887089597,
2.18433415334443));
#11876=CARTESIAN_POINT('Ctrl Pts',(-17.060764564953,-10.5074343717227,2.07319300581542));
#11877=CARTESIAN_POINT('Ctrl Pts',(-16.5439255850677,-8.54379463956336,
1.9620518582864));
#11878=CARTESIAN_POINT('Ctrl Pts',(-14.6138381736448,-7.91310778580779,
1.85091071075738));
#11879=CARTESIAN_POINT('Ctrl Pts',(-13.0372280140179,-9.19267943444714,
1.73976956322836));
#11880=CARTESIAN_POINT('Ctrl Pts',(-13.2572617631922,-11.2112406500812,
1.62862841569934));
#11881=CARTESIAN_POINT('Ctrl Pts',(-15.0725291305554,-12.1210795980947,
1.51748726817032));
#11882=CARTESIAN_POINT('Ctrl Pts',(-16.821406321826,-11.0893670397582,1.4063461206413));
#11883=CARTESIAN_POINT('Ctrl Pts',(-16.903039939412,-9.06048921956191,1.29520497311228));
#11884=CARTESIAN_POINT('Ctrl Pts',(-15.2427064949249,-7.89160580102436,
1.18406382558326));
#11885=CARTESIAN_POINT('Ctrl Pts',(-13.3602082285737,-8.65265652892044,
1.07292267805424));
#11886=CARTESIAN_POINT('Ctrl Pts',(-12.978712248134,-10.6470248895129,0.961781530525217));
#11887=CARTESIAN_POINT('Ctrl Pts',(-14.4474198117375,-12.04910765644,0.850640382996199));
#11888=CARTESIAN_POINT('Ctrl Pts',(-16.4219439272521,-11.5755659478345,
0.739499235467178));
#11889=CARTESIAN_POINT('Ctrl Pts',(-17.0948642026044,-9.65972108929999,
0.62835808793816));
#11890=CARTESIAN_POINT('Ctrl Pts',(-15.8502530039462,-8.05553312654103,
0.517216940409138));
#11891=CARTESIAN_POINT('Ctrl Pts',(-13.8273065432951,-8.2308862469267,0.40607579288012));
#11892=CARTESIAN_POINT('Ctrl Pts',(-12.8778889072789,-10.0262889388929,
0.294934645351099));
#11893=CARTESIAN_POINT('Ctrl Pts',(-13.8707906674137,-11.796321686361,0.183793497822079));
#11894=CARTESIAN_POINT('Ctrl Pts',(-15.8976661543735,-11.9246251143613,
0.07265235029306));
#11895=CARTESIAN_POINT('Ctrl Pts',(-17.102226890173,-10.2860459063565,-0.0384887972359602));
#11896=CARTESIAN_POINT('Ctrl Pts',(-16.6230126406787,-9.02713415977149,
-0.11258289558864));
#11897=CARTESIAN_POINT('Ctrl Pts',(-16.170112749004,-8.63803243006198,-0.14962994476498));
#11898=CARTESIAN_POINT('Ctrl Pts',(-13.5335096305347,-8.75273391342904,
8.14962994476498));
#11899=CARTESIAN_POINT('Ctrl Pts',(-13.1187518286854,-9.24039114120217,
8.11258289558864));
#11900=CARTESIAN_POINT('Ctrl Pts',(-12.8212320921502,-10.6536622167997,
8.03848879723595));
#11901=CARTESIAN_POINT('Ctrl Pts',(-14.3703529517921,-12.1881434126541,
7.92734764970695));
#11902=CARTESIAN_POINT('Ctrl Pts',(-16.4956311995161,-11.7141183788172,
7.81620650217792));
#11903=CARTESIAN_POINT('Ctrl Pts',(-17.2519333559009,-9.67381730766822,
7.7050653546489));
#11904=CARTESIAN_POINT('Ctrl Pts',(-15.9468745321282,-7.93067812439536,
7.59392420711988));
#11905=CARTESIAN_POINT('Ctrl Pts',(-13.7750994238661,-8.08244220797005,
7.48278305959086));
#11906=CARTESIAN_POINT('Ctrl Pts',(-12.7245420559471,-9.9890874663089,7.37164191206184));
#11907=CARTESIAN_POINT('Ctrl Pts',(-13.756852958811,-11.9059153129918,7.26050076453282));
#11908=CARTESIAN_POINT('Ctrl Pts',(-15.9270894349734,-12.0780437016018,
7.1493596170038));
#11909=CARTESIAN_POINT('Ctrl Pts',(-17.2487059684241,-10.3480646035229,
7.03821846947478));
#11910=CARTESIAN_POINT('Ctrl Pts',(-16.5119454092653,-8.29945432541285,
6.92707732194576));
#11911=CARTESIAN_POINT('Ctrl Pts',(-14.3912100840495,-7.80747005132744,
6.81593617441674));
#11912=CARTESIAN_POINT('Ctrl Pts',(-12.8277368315367,-9.32243392681855,
6.70479502688772));
#11913=CARTESIAN_POINT('Ctrl Pts',(-13.252667477277,-11.4576186515678,6.59365387935869));
#11914=CARTESIAN_POINT('Ctrl Pts',(-15.2770371928816,-12.2585550055097,
6.48251273182969));
#11915=CARTESIAN_POINT('Ctrl Pts',(-17.0478180352521,-10.9921003739429,
6.37137158430066));
#11916=CARTESIAN_POINT('Ctrl Pts',(-16.9441071998576,-8.81751578167622,
6.26023043677165));
#11917=CARTESIAN_POINT('Ctrl Pts',(-15.0608375009569,-7.72533075134102,
6.14908928924262));
#11918=CARTESIAN_POINT('Ctrl Pts',(-13.1218795561602,-8.71528788672682,
6.03794814171361));
#11919=CARTESIAN_POINT('Ctrl Pts',(-12.9020788140733,-10.8812197674026,
5.92680699418457));
#11920=CARTESIAN_POINT('Ctrl Pts',(-14.6026321818275,-12.2405178771688,
5.81566584665556));
#11921=CARTESIAN_POINT('Ctrl Pts',(-16.6669203404595,-11.5489345212182,
5.70452469912655));
#11922=CARTESIAN_POINT('Ctrl Pts',(-17.205375522286,-9.43951773345887,5.59338355159752));
#11923=CARTESIAN_POINT('Ctrl Pts',(-15.7251171424241,-7.84314425825552,
5.4822424040685));
#11924=CARTESIAN_POINT('Ctrl Pts',(-13.5811151984292,-8.22107125348279,
5.37110125653949));
#11925=CARTESIAN_POINT('Ctrl Pts',(-12.7359043050575,-10.2273592931811,
5.25996010901046));
#11926=CARTESIAN_POINT('Ctrl Pts',(-13.9631570979619,-12.0255316240646,
5.14881896148144));
#11927=CARTESIAN_POINT('Ctrl Pts',(-16.1394948909739,-11.9696123876616,
5.03767781395243));
#11928=CARTESIAN_POINT('Ctrl Pts',(-17.2727841116396,-10.1107878416383,
4.92653666642339));
#11929=CARTESIAN_POINT('Ctrl Pts',(-16.3256566128762,-8.15055248555867,
4.81539551889439));
#11930=CARTESIAN_POINT('Ctrl Pts',(-14.1650754615946,-7.88322826474304,
4.70425437136536));
#11931=CARTESIAN_POINT('Ctrl Pts',(-12.7687512233509,-9.55351320211825,
4.59311322383635));
#11932=CARTESIAN_POINT('Ctrl Pts',(-13.4148239010208,-11.6324945020439,
4.48197207630732));
#11933=CARTESIAN_POINT('Ctrl Pts',(-15.5119041084733,-12.2171548767998,
4.37083092877831));
#11934=CARTESIAN_POINT('Ctrl Pts',(-17.1404075335735,-10.7723193343466,
4.25968978124929));
#11935=CARTESIAN_POINT('Ctrl Pts',(-16.809666525189,-8.62053320750586,4.14854863372026));
#11936=CARTESIAN_POINT('Ctrl Pts',(-14.8224283262808,-7.73145644417431,
4.03740748619125));
#11937=CARTESIAN_POINT('Ctrl Pts',(-12.997732217055,-8.9189147631365,3.92626633866222));
#11938=CARTESIAN_POINT('Ctrl Pts',(-13.0058328750556,-11.0959557663405,
3.81512519113321));
#11939=CARTESIAN_POINT('Ctrl Pts',(-14.8393152782154,-12.2698021905386,
3.70398404360418));
#11940=CARTESIAN_POINT('Ctrl Pts',(-16.8198821228955,-11.3659614279855,
3.59284289607517));
#11941=CARTESIAN_POINT('Ctrl Pts',(-17.1346008227942,-9.21177357865423,
3.48170174854615));
#11942=CARTESIAN_POINT('Ctrl Pts',(-15.4953903226807,-7.77909703223927,
3.37056060101712));
#11943=CARTESIAN_POINT('Ctrl Pts',(-13.402719106847,-8.3793472573361,3.25941945348811));
#11944=CARTESIAN_POINT('Ctrl Pts',(-12.7721356708031,-10.4630789291993,
3.14827830595908));
#11945=CARTESIAN_POINT('Ctrl Pts',(-14.1808511612947,-12.1229264575659,
3.03713715843007));
#11946=CARTESIAN_POINT('Ctrl Pts',(-16.339383112999,-11.8395310381196,2.92599601090104));
#11947=CARTESIAN_POINT('Ctrl Pts',(-17.2718967167089,-9.87230163407375,
2.81485486337203));
#11948=CARTESIAN_POINT('Ctrl Pts',(-16.1248058871327,-8.02196226487325,
2.703713715843));
#11949=CARTESIAN_POINT('Ctrl Pts',(-13.9481122187642,-7.98224043637001,
2.59257256831399));
#11950=CARTESIAN_POINT('Ctrl Pts',(-12.7342750377617,-9.78949593615416,
2.48143142078496));
#11951=CARTESIAN_POINT('Ctrl Pts',(-13.5943929105772,-11.7894385383755,
2.37029027325595));
#11952=CARTESIAN_POINT('Ctrl Pts',(-15.741147939955,-12.1513998400885,2.25914912572692));
#11953=CARTESIAN_POINT('Ctrl Pts',(-17.2094854494613,-10.5440548037099,
2.14800797819791));
#11954=CARTESIAN_POINT('Ctrl Pts',(-16.6553473275274,-8.43870347441375,
2.03686683066889));
#11955=CARTESIAN_POINT('Ctrl Pts',(-14.5859697167838,-7.76250132583336,
1.92572568313987));
#11956=CARTESIAN_POINT('Ctrl Pts',(-12.8955790402303,-9.13441686984722,
1.81458453561085));
#11957=CARTESIAN_POINT('Ctrl Pts',(-13.1314921452297,-11.298653246307,1.70344338808183));
#11958=CARTESIAN_POINT('Ctrl Pts',(-15.0777633997351,-12.274153287009,1.59230224055281));
#11959=CARTESIAN_POINT('Ctrl Pts',(-16.9528532439237,-11.1679842833106,
1.48116109302379));
#11960=CARTESIAN_POINT('Ctrl Pts',(-17.0403781816632,-8.99268677543598,
1.37001994549477));
#11961=CARTESIAN_POINT('Ctrl Pts',(-15.2602220933659,-7.73944758969995,
1.25887879796575));
#11962=CARTESIAN_POINT('Ctrl Pts',(-13.2418680325108,-8.55542168891818,
1.14773765043673));
#11963=CARTESIAN_POINT('Ctrl Pts',(-12.8328403191345,-10.6937192647481,
1.03659650290771));
#11964=CARTESIAN_POINT('Ctrl Pts',(-14.4075413046253,-12.1969872872825,
0.925455355378688));
#11965=CARTESIAN_POINT('Ctrl Pts',(-16.5245625194866,-11.6892711062734,
0.814314207849668));
#11966=CARTESIAN_POINT('Ctrl Pts',(-17.2460459835971,-9.63516390239978,
0.703173060320648));
#11967=CARTESIAN_POINT('Ctrl Pts',(-15.9116139089972,-7.91520519280415,
0.592031912791628));
#11968=CARTESIAN_POINT('Ctrl Pts',(-13.7426758139511,-8.10321316547549,
0.480890765262609));
#11969=CARTESIAN_POINT('Ctrl Pts',(-12.7247407776469,-10.0281861542815,
0.369749617733589));
#11970=CARTESIAN_POINT('Ctrl Pts',(-13.7892980924765,-11.9259583050221,
0.258608470204568));
#11971=CARTESIAN_POINT('Ctrl Pts',(-15.9624487630916,-12.0635211116153,
0.147467322675549));
#11972=CARTESIAN_POINT('Ctrl Pts',(-17.2539400202709,-10.3066892156053,
0.0363261751465287));
#11973=CARTESIAN_POINT('Ctrl Pts',(-16.7401419234677,-8.95692455372168,
-0.0377679232061509));
#11974=CARTESIAN_POINT('Ctrl Pts',(-16.2545572343013,-8.53974220073755,
-0.0748149723824913));
#11975=CARTESIAN_POINT('Ctrl Pts',(-13.4347998857283,-8.66878019666781,
8.22444491714747));
#11976=CARTESIAN_POINT('Ctrl Pts',(-12.9921246576009,-9.18926172489923,
8.18739786797113));
#11977=CARTESIAN_POINT('Ctrl Pts',(-12.6745788111916,-10.6976603445429,
8.11330376961844));
#11978=CARTESIAN_POINT('Ctrl Pts',(-14.3279712896,-12.3354277606187,8.00216262208943));
#11979=CARTESIAN_POINT('Ctrl Pts',(-16.5963024191182,-11.8294960118818,
7.89102147456041));
#11980=CARTESIAN_POINT('Ctrl Pts',(-17.4035114170396,-9.65186188880512,
7.77988032703139));
#11981=CARTESIAN_POINT('Ctrl Pts',(-16.0106088364074,-7.79139167661744,
7.66873917950237));
#11982=CARTESIAN_POINT('Ctrl Pts',(-13.6926511338527,-7.95337102943111,
7.55759803197335));
#11983=CARTESIAN_POINT('Ctrl Pts',(-12.5713805503198,-9.98835294159719,
7.44645688444433));
#11984=CARTESIAN_POINT('Ctrl Pts',(-13.6731764957754,-12.0342028340593,
7.3353157369153));
#11985=CARTESIAN_POINT('Ctrl Pts',(-15.989492000612,-12.2179172171411,7.22417458938629));
#11986=CARTESIAN_POINT('Ctrl Pts',(-17.4000667934998,-10.371492897977,7.11303344185727));
#11987=CARTESIAN_POINT('Ctrl Pts',(-16.6137147414187,-8.18499027364317,
7.00189229432825));
#11988=CARTESIAN_POINT('Ctrl Pts',(-14.350232319384,-7.65989044479182,6.89075114679923));
#11989=CARTESIAN_POINT('Ctrl Pts',(-12.6815213858194,-9.27682682597027,
6.77960999927021));
#11990=CARTESIAN_POINT('Ctrl Pts',(-13.1350541938888,-11.5557312393606,
6.66846885174119));
#11991=CARTESIAN_POINT('Ctrl Pts',(-15.295684618859,-12.4105787711389,6.55732770421217));
#11992=CARTESIAN_POINT('Ctrl Pts',(-17.185657055459,-11.0588788382093,6.44618655668315));
#11993=CARTESIAN_POINT('Ctrl Pts',(-17.0749654240711,-8.73792254474896,
6.33504540915413));
#11994=CARTESIAN_POINT('Ctrl Pts',(-15.0649324846807,-7.5722223329502,6.22390426162511));
#11995=CARTESIAN_POINT('Ctrl Pts',(-12.995462913005,-8.62881367080874,6.11276311409609));
#11996=CARTESIAN_POINT('Ctrl Pts',(-12.7608673412954,-10.9405348370204,
6.00162196656707));
#11997=CARTESIAN_POINT('Ctrl Pts',(-14.5758852786477,-12.3913275602698,
5.89048081903805));
#11998=CARTESIAN_POINT('Ctrl Pts',(-16.7791210646139,-11.65319359751,5.77933967150903));
#11999=CARTESIAN_POINT('Ctrl Pts',(-17.353819766817,-9.40179156583393,5.66819852398001));
#12000=CARTESIAN_POINT('Ctrl Pts',(-15.7739249147585,-7.69796588935184,
5.55705737645099));
#12001=CARTESIAN_POINT('Ctrl Pts',(-13.4856097934235,-8.10133122228054,
5.44591622892198));
#12002=CARTESIAN_POINT('Ctrl Pts',(-12.583507594572,-10.2426628903111,5.33477508139295));
#12003=CARTESIAN_POINT('Ctrl Pts',(-13.8933670056466,-12.161870541709,5.22363393386393));
#12004=CARTESIAN_POINT('Ctrl Pts',(-16.2161945081267,-12.1021873709018,
5.11249278633491));
#12005=CARTESIAN_POINT('Ctrl Pts',(-17.4257656411002,-10.1182449922637,
5.00135163880589));
#12006=CARTESIAN_POINT('Ctrl Pts',(-16.4148868108254,-8.02606582271751,
4.89021049127687));
#12007=CARTESIAN_POINT('Ctrl Pts',(-14.1088765326179,-7.74074795791574,
4.77906934374786));
#12008=CARTESIAN_POINT('Ctrl Pts',(-12.6185654451633,-9.52346009110162,
4.66792819621883));
#12009=CARTESIAN_POINT('Ctrl Pts',(-13.3081253972587,-11.7423780164876,
4.55678704868982));
#12010=CARTESIAN_POINT('Ctrl Pts',(-15.5463604710685,-12.3663919919164,
4.44564590116079));
#12011=CARTESIAN_POINT('Ctrl Pts',(-17.2844787704667,-10.8243042951685,
4.33450475363178));
#12012=CARTESIAN_POINT('Ctrl Pts',(-16.9314755221013,-8.52768103616449,
4.22336360610275));
#12013=CARTESIAN_POINT('Ctrl Pts',(-14.8104759432562,-7.57876034732949,
4.11222245857374));
#12014=CARTESIAN_POINT('Ctrl Pts',(-12.8629591929671,-8.84614671087597,
4.00108131104471));
#12015=CARTESIAN_POINT('Ctrl Pts',(-12.8716051077936,-11.1697247567595,
3.88994016351569));
#12016=CARTESIAN_POINT('Ctrl Pts',(-14.8284995591272,-12.4225830063246,
3.77879901598667));
#12017=CARTESIAN_POINT('Ctrl Pts',(-16.9423787336263,-11.4579045506812,
3.66765786845765));
#12018=CARTESIAN_POINT('Ctrl Pts',(-17.2782812088839,-9.15871790879045,
3.55651672092864));
#12019=CARTESIAN_POINT('Ctrl Pts',(-15.5287351392234,-7.62960763240948,
3.44537557339961));
#12020=CARTESIAN_POINT('Ctrl Pts',(-13.2952058270941,-8.27026081396139,
3.33423442587059));
#12021=CARTESIAN_POINT('Ctrl Pts',(-12.6221777004152,-10.4942488597207,
3.22309327834158));
#12022=CARTESIAN_POINT('Ctrl Pts',(-14.1257140976557,-12.2658210399188,
3.11195213081255));
#12023=CARTESIAN_POINT('Ctrl Pts',(-16.429537244274,-11.9633502210594,3.00081098328354));
#12024=CARTESIAN_POINT('Ctrl Pts',(-17.4248185154485,-9.8637062328524,2.88966983575451));
#12025=CARTESIAN_POINT('Ctrl Pts',(-16.2005167846521,-7.88882016989784,
2.77852868822549));
#12026=CARTESIAN_POINT('Ctrl Pts',(-13.8773094527777,-7.84642465758702,
2.66738754069648));
#12027=CARTESIAN_POINT('Ctrl Pts',(-12.5817686609856,-9.7753268677064,2.55624639316746));
#12028=CARTESIAN_POINT('Ctrl Pts',(-13.4997812308935,-11.9098859856603,
2.44510524563844));
#12029=CARTESIAN_POINT('Ctrl Pts',(-15.7910347483105,-12.2962109712173,
2.33396409810941));
#12030=CARTESIAN_POINT('Ctrl Pts',(-17.3582063339697,-10.5806752356971,
2.2228229505804));
#12031=CARTESIAN_POINT('Ctrl Pts',(-16.7667690699872,-8.33361230926411,
2.11168180305138));
#12032=CARTESIAN_POINT('Ctrl Pts',(-14.5581012599229,-7.61189486585896,
2.00054065552235));
#12033=CARTESIAN_POINT('Ctrl Pts',(-12.7539300664426,-9.07615430524727,
1.88939950799334));
#12034=CARTESIAN_POINT('Ctrl Pts',(-13.0057225272674,-11.3860658425327,
1.77825836046431));
#12035=CARTESIAN_POINT('Ctrl Pts',(-15.0829976689147,-12.4272269759234,
1.6671172129353));
#12036=CARTESIAN_POINT('Ctrl Pts',(-17.0843001660214,-11.2466015268631,
1.55597606540628));
#12037=CARTESIAN_POINT('Ctrl Pts',(-17.1777164239143,-8.92488433131005,
1.44483491787726));
#12038=CARTESIAN_POINT('Ctrl Pts',(-15.2777376918069,-7.58728937837554,
1.33369377034824));
#12039=CARTESIAN_POINT('Ctrl Pts',(-13.1235278364479,-8.45818684891592,
1.22255262281922));
#12040=CARTESIAN_POINT('Ctrl Pts',(-12.686968390135,-10.7404136399833,1.1114114752902));
#12041=CARTESIAN_POINT('Ctrl Pts',(-14.367662797513,-12.344866918125,1.00027032776118));
#12042=CARTESIAN_POINT('Ctrl Pts',(-16.6271811117211,-11.8029762647123,
0.889129180232156));
#12043=CARTESIAN_POINT('Ctrl Pts',(-17.3972277645898,-9.61060671549959,
0.777988032703138));
#12044=CARTESIAN_POINT('Ctrl Pts',(-15.9729748140483,-7.77487725906727,
0.666846885174117));
#12045=CARTESIAN_POINT('Ctrl Pts',(-13.6580450846071,-7.97554008402429,
0.555705737645098));
#12046=CARTESIAN_POINT('Ctrl Pts',(-12.5715926480149,-10.0300833696701,
0.444564590116077));
#12047=CARTESIAN_POINT('Ctrl Pts',(-13.7078055175393,-12.0555949236832,
0.333423442587058));
#12048=CARTESIAN_POINT('Ctrl Pts',(-16.0272313718098,-12.2024171088693,
0.222282295058038));
#12049=CARTESIAN_POINT('Ctrl Pts',(-17.4056531503688,-10.3273325248541,
0.111141147529018));
#12050=CARTESIAN_POINT('Ctrl Pts',(-16.8572712062568,-8.88671494767186,
0.0370470491763382));
#12051=CARTESIAN_POINT('Ctrl Pts',(-16.3390017195986,-8.44145197141311,
-2.22044604925031E-15));
#12052=CARTESIAN_POINT('Ctrl Pts',(-16.3390017195986,-8.44145197141311,
-2.22044604925031E-15));
#12053=CARTESIAN_POINT('Ctrl Pts',(-16.3898412550158,-8.49415674362063,
-2.22613706717393E-15));
#12054=CARTESIAN_POINT('Ctrl Pts',(-16.4374589296418,-8.54962581051277,
-1.71409610791473E-15));
#12055=CARTESIAN_POINT('Ctrl Pts',(-16.4818118062285,-8.60751256073212,
-1.85962356624714E-15));
#12056=CARTESIAN_POINT('Ctrl Pts',(-16.5273944148942,-8.66700428449924,
-2.00918593274442E-15));
#12057=CARTESIAN_POINT('Ctrl Pts',(-16.5695290717974,-8.7290505709106,-1.66395111688824E-15));
#12058=CARTESIAN_POINT('Ctrl Pts',(-16.6081216798471,-8.79330183658361,
-1.58206781009085E-15));
#12059=CARTESIAN_POINT('Ctrl Pts',(-16.640731850897,-8.84759318587709,-1.51287765229278E-15));
#12060=CARTESIAN_POINT('Ctrl Pts',(-16.6708122443294,-8.90345969057086,
-3.85227514727774E-17));
#12061=CARTESIAN_POINT('Ctrl Pts',(-16.6982777801774,-8.96069680171699,
-1.38777878078145E-16));
#12062=CARTESIAN_POINT('Ctrl Pts',(-16.7104763391781,-8.98611812541558,
-1.83305248080649E-16));
#12063=CARTESIAN_POINT('Ctrl Pts',(-16.7221587384426,-9.01180984573392,
-1.61721416497441E-15));
#12064=CARTESIAN_POINT('Ctrl Pts',(-16.7333158123914,-9.0377540202666,-1.74860126378462E-15));
#12065=CARTESIAN_POINT('Ctrl Pts',(-16.7394484186841,-9.05201451622892,
-1.82081960280802E-15));
#12066=CARTESIAN_POINT('Ctrl Pts',(-16.7454222912401,-9.06635128371498,
-1.59328855671869E-15));
#12067=CARTESIAN_POINT('Ctrl Pts',(-16.7512357689513,-9.08076132240649,
-1.66533453693773E-15));
#12068=CARTESIAN_POINT('Ctrl Pts',(-16.7565954716119,-9.09404657549439,
-1.73175691800603E-15));
#12069=CARTESIAN_POINT('Ctrl Pts',(-16.761819475366,-9.10739609302559,-3.43152104970979E-15));
#12070=CARTESIAN_POINT('Ctrl Pts',(-16.7668988698636,-9.12078671142655,
-3.3584246494911E-15));
#12071=CARTESIAN_POINT('Ctrl Pts',(-16.792860351532,-9.18922799794368,-2.98481892636936E-15));
#12072=CARTESIAN_POINT('Ctrl Pts',(-16.8150968550578,-9.2588588983408,3.9807706675476E-16));
#12073=CARTESIAN_POINT('Ctrl Pts',(-16.833523678901,-9.32935115717727,4.9960036108132E-16));
#12074=CARTESIAN_POINT('Ctrl Pts',(-16.851806919093,-9.39929413329465,6.00332575761995E-16));
#12075=CARTESIAN_POINT('Ctrl Pts',(-16.8663396941486,-9.47008611206394,
-1.23947449676468E-16));
#12076=CARTESIAN_POINT('Ctrl Pts',(-16.8769883967272,-9.54140886116961,
3.88578058618805E-16));
#12077=CARTESIAN_POINT('Ctrl Pts',(-16.8858394571407,-9.60069138470125,
8.14582466568122E-16));
#12078=CARTESIAN_POINT('Ctrl Pts',(-16.8920062609022,-9.66034091039286,
-3.79887144988971E-15));
#12079=CARTESIAN_POINT('Ctrl Pts',(-16.8953843819236,-9.72016855746037,
-4.21884749357559E-15));
#12080=CARTESIAN_POINT('Ctrl Pts',(-16.8967942299417,-9.74513743486574,
-4.39412315394293E-15));
#12081=CARTESIAN_POINT('Ctrl Pts',(-16.897718042808,-9.77013723287953,-1.04049734037864E-15));
#12082=CARTESIAN_POINT('Ctrl Pts',(-16.8981468950099,-9.79515367142193,
-1.16573417585641E-15));
#12083=CARTESIAN_POINT('Ctrl Pts',(-16.8983454979286,-9.80673886950697,
-1.22373178187433E-15));
#12084=CARTESIAN_POINT('Ctrl Pts',(-16.8984379380574,-9.81832763098025,
-2.19002109012887E-15));
#12085=CARTESIAN_POINT('Ctrl Pts',(-16.8984232708294,-9.82991850741629,
-2.35922392732846E-15));
#12086=CARTESIAN_POINT('Ctrl Pts',(-16.898407987489,-9.8419962708459,-2.53553430822076E-15));
#12087=CARTESIAN_POINT('Ctrl Pts',(-16.898276391407,-9.85406801930843,2.2754508191584E-15));
#12088=CARTESIAN_POINT('Ctrl Pts',(-16.8980280297643,-9.86612772948922,
2.24820162486594E-15));
#12089=CARTESIAN_POINT('Ctrl Pts',(-16.896612869921,-9.93484372517432,2.09293624208695E-15));
#12090=CARTESIAN_POINT('Ctrl Pts',(-16.8914106127702,-10.0032167380162,
-1.36002320516582E-15));
#12091=CARTESIAN_POINT('Ctrl Pts',(-16.8823084122723,-10.0709659878617,
-1.36002320516582E-15));
#12092=CARTESIAN_POINT('Ctrl Pts',(-16.874055619439,-10.1323929498053,-1.36002320516582E-15));
#12093=CARTESIAN_POINT('Ctrl Pts',(-16.862596252108,-10.1933075358049,-1.26372848136827E-15));
#12094=CARTESIAN_POINT('Ctrl Pts',(-16.8478109454459,-10.2534888721422,
-1.38777878078145E-15));
#12095=CARTESIAN_POINT('Ctrl Pts',(-16.8303241431413,-10.3246662345746,
-1.52144137683588E-15));
#12096=CARTESIAN_POINT('Ctrl Pts',(-16.8081848462467,-10.3948195464577,
1.0568803955417E-15));
#12097=CARTESIAN_POINT('Ctrl Pts',(-16.7816446910013,-10.4635997456855,
9.15933995315754E-16));
#12098=CARTESIAN_POINT('Ctrl Pts',(-16.7758002954335,-10.47874580221,8.84896252350212E-16));
#12099=CARTESIAN_POINT('Ctrl Pts',(-16.7697423260011,-10.4938251023906,
3.43889358474875E-15));
#12100=CARTESIAN_POINT('Ctrl Pts',(-16.76347320795,-10.5088336097722,3.58046925441613E-15));
#12101=CARTESIAN_POINT('Ctrl Pts',(-16.757017516591,-10.5242887807586,3.72625831435445E-15));
#12102=CARTESIAN_POINT('Ctrl Pts',(-16.7503352761988,-10.5396743969356,
1.17227682962454E-15));
#12103=CARTESIAN_POINT('Ctrl Pts',(-16.7434433794614,-10.5549551926611,
1.11022302462516E-15));
#12104=CARTESIAN_POINT('Ctrl Pts',(-16.7152442624164,-10.6174786116301,
8.56321583999907E-16));
#12105=CARTESIAN_POINT('Ctrl Pts',(-16.6835079213234,-10.678330876987,-5.09021181669685E-16));
#12106=CARTESIAN_POINT('Ctrl Pts',(-16.6484901027957,-10.7372591681392,
-6.24500451351651E-16));
#12107=CARTESIAN_POINT('Ctrl Pts',(-16.6134795778401,-10.7961751856045,
-7.39955668810536E-16));
#12108=CARTESIAN_POINT('Ctrl Pts',(-16.5751880678017,-10.8531687996888,
-5.44190642062304E-16));
#12109=CARTESIAN_POINT('Ctrl Pts',(-16.5338329814792,-10.9079522899894,
-1.36002320516582E-15));
#12110=CARTESIAN_POINT('Ctrl Pts',(-16.5038966901276,-10.9476091900891,
-1.95059146351222E-15));
#12111=CARTESIAN_POINT('Ctrl Pts',(-16.4723542281424,-10.9861072729443,
3.54640415640727E-16));
#12112=CARTESIAN_POINT('Ctrl Pts',(-16.4392794411118,-11.023322519061,4.23272528138341E-16));
#12113=CARTESIAN_POINT('Ctrl Pts',(-16.4144728570297,-11.0512345092751,
4.74747637194398E-16));
#12114=CARTESIAN_POINT('Ctrl Pts',(-16.3888041482335,-11.078424626853,-2.43914533858063E-18));
#12115=CARTESIAN_POINT('Ctrl Pts',(-16.3623027552176,-11.1048350815606,
-1.2490009027033E-16));
#12116=CARTESIAN_POINT('Ctrl Pts',(-16.3534958039143,-11.1136118122165,
-1.65596350195737E-16));
#12117=CARTESIAN_POINT('Ctrl Pts',(-16.344603778745,-11.1222955249443,1.47368254087686E-15));
#12118=CARTESIAN_POINT('Ctrl Pts',(-16.3356283270931,-11.1308842376674,
1.38083988687754E-15));
#12119=CARTESIAN_POINT('Ctrl Pts',(-16.288023609681,-11.1764377382574,8.88413602512318E-16));
#12120=CARTESIAN_POINT('Ctrl Pts',(-16.2380710211992,-11.2193250402242,
1.04010533930317E-15));
#12121=CARTESIAN_POINT('Ctrl Pts',(-16.1859608069979,-11.2592665759842,
1.45716771982052E-15));
#12122=CARTESIAN_POINT('Ctrl Pts',(-16.1492839781811,-11.2873787012596,
1.75070950947919E-15));
#12123=CARTESIAN_POINT('Ctrl Pts',(-16.1115377653254,-11.3140307077825,
1.50961177331903E-15));
#12124=CARTESIAN_POINT('Ctrl Pts',(-16.0727840466388,-11.3391103479433,
1.30104260698261E-15));
#12125=CARTESIAN_POINT('Ctrl Pts',(-16.0603479160929,-11.3471584447364,
1.23411242664593E-15));
#12126=CARTESIAN_POINT('Ctrl Pts',(-16.0478062717038,-11.3550455819844,
3.29476744426013E-15));
#12127=CARTESIAN_POINT('Ctrl Pts',(-16.035166679802,-11.3627643666854,3.46944695195361E-15));
#12128=CARTESIAN_POINT('Ctrl Pts',(-15.9813223879855,-11.3956461637514,
4.21357654567057E-15));
#12129=CARTESIAN_POINT('Ctrl Pts',(-15.9258102639214,-11.4254113967777,
2.49285835226939E-15));
#12130=CARTESIAN_POINT('Ctrl Pts',(-15.8687981257942,-11.4517907020109,
7.73686670285656E-16));
#12131=CARTESIAN_POINT('Ctrl Pts',(-15.8162031923817,-11.4761261829765,
-8.1228647698802E-16));
#12132=CARTESIAN_POINT('Ctrl Pts',(-15.7623311074045,-11.4975799204738,
-1.81768923500598E-15));
#12133=CARTESIAN_POINT('Ctrl Pts',(-15.7073085825,-11.5159013381686,-2.16320017454308E-15));
#12134=CARTESIAN_POINT('Ctrl Pts',(-15.6970482491915,-11.5193178271894,
-2.23227875911951E-15));
#12135=CARTESIAN_POINT('Ctrl Pts',(-15.6867479087967,-11.522625281403,-1.49184837699714E-15));
#12136=CARTESIAN_POINT('Ctrl Pts',(-15.6764092460937,-11.5258237909713,
-1.51267887105178E-15));
#12137=CARTESIAN_POINT('Ctrl Pts',(-13.1992962903993,-10.0024064022658,
8.));
#12138=CARTESIAN_POINT('Ctrl Pts',(-13.1914749172297,-10.0697907508692,
8.));
#12139=CARTESIAN_POINT('Ctrl Pts',(-13.187400594648,-10.13757275596,8.));
#12140=CARTESIAN_POINT('Ctrl Pts',(-13.1871885483144,-10.2054359876388,
8.));
#12141=CARTESIAN_POINT('Ctrl Pts',(-13.1871289997272,-10.2244938958915,
8.));
#12142=CARTESIAN_POINT('Ctrl Pts',(-13.1873743545316,-10.243558269923,8.));
#12143=CARTESIAN_POINT('Ctrl Pts',(-13.1879279070141,-10.2626221926416,
8.));
#12144=CARTESIAN_POINT('Ctrl Pts',(-13.1882788291768,-10.2747076826339,
8.));
#12145=CARTESIAN_POINT('Ctrl Pts',(-13.188753786007,-10.2867946010088,8.));
#12146=CARTESIAN_POINT('Ctrl Pts',(-13.1893525572532,-10.2988636614694,
8.));
#12147=CARTESIAN_POINT('Ctrl Pts',(-13.1928456546243,-10.3692718576439,
8.));
#12148=CARTESIAN_POINT('Ctrl Pts',(-13.200551400234,-10.4392065520031,8.));
#12149=CARTESIAN_POINT('Ctrl Pts',(-13.2125313402152,-10.5083097512027,
8.));
#12150=CARTESIAN_POINT('Ctrl Pts',(-13.2141825349725,-10.5178342430122,
8.));
#12151=CARTESIAN_POINT('Ctrl Pts',(-13.2159150020402,-10.527342969275,8.));
#12152=CARTESIAN_POINT('Ctrl Pts',(-13.2177289760061,-10.5368350182323,
8.));
#12153=CARTESIAN_POINT('Ctrl Pts',(-13.2303840186811,-10.6030555301501,
8.));
#12154=CARTESIAN_POINT('Ctrl Pts',(-13.2470016652037,-10.6684641941904,
8.));
#12155=CARTESIAN_POINT('Ctrl Pts',(-13.2673108671637,-10.732853414775,8.));
#12156=CARTESIAN_POINT('Ctrl Pts',(-13.2891629308514,-10.8021341945802,
8.));
#12157=CARTESIAN_POINT('Ctrl Pts',(-13.3152885233548,-10.8702357394381,
8.));
#12158=CARTESIAN_POINT('Ctrl Pts',(-13.3454140237584,-10.9368936728771,
8.));
#12159=CARTESIAN_POINT('Ctrl Pts',(-13.3509664607591,-10.9491794099123,
8.));
#12160=CARTESIAN_POINT('Ctrl Pts',(-13.3566549432153,-10.9614160670129,
8.));
#12161=CARTESIAN_POINT('Ctrl Pts',(-13.3624779793227,-10.9736019244815,
8.));
#12162=CARTESIAN_POINT('Ctrl Pts',(-13.3674124355839,-10.9839282524614,
8.));
#12163=CARTESIAN_POINT('Ctrl Pts',(-13.3724393907479,-10.9942094580485,
8.));
#12164=CARTESIAN_POINT('Ctrl Pts',(-13.3775570341231,-11.004443789421,8.));
#12165=CARTESIAN_POINT('Ctrl Pts',(-13.4093429320592,-11.0680096514008,
8.));
#12166=CARTESIAN_POINT('Ctrl Pts',(-13.4446277894419,-11.1297776805203,
8.));
#12167=CARTESIAN_POINT('Ctrl Pts',(-13.4831035148986,-11.1895235034675,
8.));
#12168=CARTESIAN_POINT('Ctrl Pts',(-13.5223919592831,-11.2505313314996,
8.));
#12169=CARTESIAN_POINT('Ctrl Pts',(-13.5650078538732,-11.3094314878199,
8.));
#12170=CARTESIAN_POINT('Ctrl Pts',(-13.6106776763614,-11.365976797792,8.));
#12171=CARTESIAN_POINT('Ctrl Pts',(-13.6566254157242,-11.4228662057914,
8.));
#12172=CARTESIAN_POINT('Ctrl Pts',(-13.7056649005089,-11.4773729508705,
8.));
#12173=CARTESIAN_POINT('Ctrl Pts',(-13.7575651962072,-11.5292234094565,
8.));
#12174=CARTESIAN_POINT('Ctrl Pts',(-13.770395915342,-11.5420418079294,8.));
#12175=CARTESIAN_POINT('Ctrl Pts',(-13.7834016831258,-11.5546977194546,
8.));
#12176=CARTESIAN_POINT('Ctrl Pts',(-13.7965793954044,-11.5671867011474,
8.));
#12177=CARTESIAN_POINT('Ctrl Pts',(-13.8068738937706,-11.5769431595457,
8.));
#12178=CARTESIAN_POINT('Ctrl Pts',(-13.8172745884826,-11.5865987303042,
8.));
#12179=CARTESIAN_POINT('Ctrl Pts',(-13.8277639078832,-11.5961370139814,
8.));
#12180=CARTESIAN_POINT('Ctrl Pts',(-13.8835125900578,-11.6468311271936,
8.));
#12181=CARTESIAN_POINT('Ctrl Pts',(-13.941858687196,-11.6943084473716,8.));
#12182=CARTESIAN_POINT('Ctrl Pts',(-14.0025044412164,-11.7383154250973,
8.));
#12183=CARTESIAN_POINT('Ctrl Pts',(-14.0632169827124,-11.7823708664787,
8.));
#12184=CARTESIAN_POINT('Ctrl Pts',(-14.1262348879421,-11.8229492486321,
8.));
#12185=CARTESIAN_POINT('Ctrl Pts',(-14.1913041337018,-11.8597697342368,
8.));
#12186=CARTESIAN_POINT('Ctrl Pts',(-14.2548907820865,-11.8957512681268,
8.));
#12187=CARTESIAN_POINT('Ctrl Pts',(-14.320437088868,-11.9281449399806,8.));
#12188=CARTESIAN_POINT('Ctrl Pts',(-14.3877383201204,-11.9566513247419,
8.));
#12189=CARTESIAN_POINT('Ctrl Pts',(-14.4022443265699,-11.9627955481611,
8.));
#12190=CARTESIAN_POINT('Ctrl Pts',(-14.4168319601953,-11.9687590163805,
8.));
#12191=CARTESIAN_POINT('Ctrl Pts',(-14.4314993237549,-11.9745384454386,
8.));
#12192=CARTESIAN_POINT('Ctrl Pts',(-14.4438535969467,-11.9794064399618,
8.));
#12193=CARTESIAN_POINT('Ctrl Pts',(-14.4562644367296,-11.9841438631167,
8.));
#12194=CARTESIAN_POINT('Ctrl Pts',(-14.4687300448211,-11.9887511357905,
8.));
#12195=CARTESIAN_POINT('Ctrl Pts',(-13.7309291201476,-8.92064134695149,
8.));
#12196=CARTESIAN_POINT('Ctrl Pts',(-13.6852992237889,-8.96320919740821,
8.));
#12197=CARTESIAN_POINT('Ctrl Pts',(-13.6424343385012,-9.00837891446438,
8.));
#12198=CARTESIAN_POINT('Ctrl Pts',(-13.6023333218234,-9.05579903672846,
8.));
#12199=CARTESIAN_POINT('Ctrl Pts',(-13.5611744803124,-9.10447005453275,
8.));
#12200=CARTESIAN_POINT('Ctrl Pts',(-13.5229267493543,-9.15551228037441,
8.));
#12201=CARTESIAN_POINT('Ctrl Pts',(-13.4876147577988,-9.20859491497877,
8.));
#12202=CARTESIAN_POINT('Ctrl Pts',(-13.4504234878807,-9.26450256857094,
8.));
#12203=CARTESIAN_POINT('Ctrl Pts',(-13.4164879292609,-9.32267412786545,
8.));
#12204=CARTESIAN_POINT('Ctrl Pts',(-13.3858756344612,-9.38276912102125,
8.));
#12205=CARTESIAN_POINT('Ctrl Pts',(-13.3760567911501,-9.40204449143826,
8.));
#12206=CARTESIAN_POINT('Ctrl Pts',(-13.3665801818845,-9.42151804589282,
8.));
#12207=CARTESIAN_POINT('Ctrl Pts',(-13.3574490403934,-9.44117931849771,
8.));
#12208=CARTESIAN_POINT('Ctrl Pts',(-13.3522109746218,-9.45245797836281,
8.));
#12209=CARTESIAN_POINT('Ctrl Pts',(-13.3470863249925,-9.46379928849863,
8.));
#12210=CARTESIAN_POINT('Ctrl Pts',(-13.3420822593818,-9.47518585358561,
8.));
#12211=CARTESIAN_POINT('Ctrl Pts',(-13.315074917903,-9.53664005412922,8.));
#12212=CARTESIAN_POINT('Ctrl Pts',(-13.2915286665307,-9.59951131295569,
8.));
#12213=CARTESIAN_POINT('Ctrl Pts',(-13.2714786288552,-9.66344604206431,
8.));
#12214=CARTESIAN_POINT('Ctrl Pts',(-13.251118980486,-9.72836804492028,8.));
#12215=CARTESIAN_POINT('Ctrl Pts',(-13.2343637932416,-9.79438749311294,
8.));
#12216=CARTESIAN_POINT('Ctrl Pts',(-13.2212910825401,-9.86116786571081,
8.));
#12217=CARTESIAN_POINT('Ctrl Pts',(-13.2148890447258,-9.89387190700605,
8.));
#12218=CARTESIAN_POINT('Ctrl Pts',(-13.2093708532485,-9.92675886633403,
8.));
#12219=CARTESIAN_POINT('Ctrl Pts',(-13.2047498322757,-9.95979108763484,
8.));
#12220=CARTESIAN_POINT('Ctrl Pts',(-13.2027644288902,-9.97398325087913,
8.));
#12221=CARTESIAN_POINT('Ctrl Pts',(-13.2009464686606,-9.98818943744355,
8.));
#12222=CARTESIAN_POINT('Ctrl Pts',(-13.1992962903989,-10.0024064022693,
8.));
#12223=CARTESIAN_POINT('Ctrl Pts',(-16.6673099838652,-10.001299617498,6.87148036339021));
#12224=CARTESIAN_POINT('Ctrl Pts',(-16.6680396077119,-10.0863816229506,
6.87718308383008));
#12225=CARTESIAN_POINT('Ctrl Pts',(-16.6620894467177,-10.1713612071089,
6.88288580426994));
#12226=CARTESIAN_POINT('Ctrl Pts',(-16.6491047202909,-10.2552518596557,
6.8885885247098));
#12227=CARTESIAN_POINT('Ctrl Pts',(-16.5647509800805,-10.8002375665841,
6.92563557388614));
#12228=CARTESIAN_POINT('Ctrl Pts',(-16.1835176418883,-11.2992671185536,
6.96268262306248));
#12229=CARTESIAN_POINT('Ctrl Pts',(-15.6798879029899,-11.5239558279272,
6.99972967223882));
#12230=CARTESIAN_POINT('Ctrl Pts',(-15.1762581640915,-11.7486445373009,
7.03677672141516));
#12231=CARTESIAN_POINT('Ctrl Pts',(-14.5502320244869,-11.6989924040788,
7.0738237705915));
#12232=CARTESIAN_POINT('Ctrl Pts',(-14.0883288184045,-11.3977023782804,
7.11087081976784));
#12233=CARTESIAN_POINT('Ctrl Pts',(-13.6264256123221,-11.0964123524819,
7.14791786894418));
#12234=CARTESIAN_POINT('Ctrl Pts',(-13.3286453397619,-10.5434844341071,
7.18496491812052));
#12235=CARTESIAN_POINT('Ctrl Pts',(-13.3312770262637,-9.99202514980564,
7.22201196729686));
#12236=CARTESIAN_POINT('Ctrl Pts',(-13.3339087127654,-9.44056586550417,
7.2590590164732));
#12237=CARTESIAN_POINT('Ctrl Pts',(-13.6369523583291,-8.89057521527605,
7.29610606564954));
#12238=CARTESIAN_POINT('Ctrl Pts',(-14.1017091677237,-8.59369096597919,
7.33315311482588));
#12239=CARTESIAN_POINT('Ctrl Pts',(-14.5664659771184,-8.29680671668234,
7.37020016400222));
#12240=CARTESIAN_POINT('Ctrl Pts',(-15.192935950344,-8.25302886831675,7.40724721317856));
#12241=CARTESIAN_POINT('Ctrl Pts',(-15.6943994886325,-8.48255279837451,
7.4442942623549));
#12242=CARTESIAN_POINT('Ctrl Pts',(-16.195863026921,-8.71207672843227,7.48134131153124));
#12243=CARTESIAN_POINT('Ctrl Pts',(-16.5723201302723,-9.21490243691337,
7.51838836070758));
#12244=CARTESIAN_POINT('Ctrl Pts',(-16.6514672697293,-9.76058778570281,
7.55543540988392));
#12245=CARTESIAN_POINT('Ctrl Pts',(-16.6628933904863,-9.83936595423039,
7.56078372771935));
#12246=CARTESIAN_POINT('Ctrl Pts',(-16.6681231513107,-9.9190373782495,7.56613204555478));
#12247=CARTESIAN_POINT('Ctrl Pts',(-16.6674570171079,-9.99879340680734,
7.57148036339021));
#12248=CARTESIAN_POINT('Ctrl Pts',(-15.5301702171886,-11.9851743256717,
8.));
#12249=CARTESIAN_POINT('Ctrl Pts',(-16.1903072548812,-11.8088749487748,
7.96295295082366));
#12250=CARTESIAN_POINT('Ctrl Pts',(-17.3094427799721,-10.7488569090756,
7.88885885247098));
#12251=CARTESIAN_POINT('Ctrl Pts',(-16.8810965229137,-8.46138998352444,
7.77771770494196));
#12252=CARTESIAN_POINT('Ctrl Pts',(-14.727662200004,-7.58731060863186,7.66657655741293));
#12253=CARTESIAN_POINT('Ctrl Pts',(-12.8251332301876,-8.91924943693317,
7.55543540988393));
#12254=CARTESIAN_POINT('Ctrl Pts',(-12.9125601407559,-11.2417229038903,
7.4442942623549));
#12255=CARTESIAN_POINT('Ctrl Pts',(-14.9111754350777,-12.4269243298781,
7.33315311482589));
#12256=CARTESIAN_POINT('Ctrl Pts',(-16.9908762005917,-11.3909493725631,
7.22201196729686));
#12257=CARTESIAN_POINT('Ctrl Pts',(-17.2483216335285,-9.08158193933239,
7.11087081976785));
#12258=CARTESIAN_POINT('Ctrl Pts',(-15.4476835001917,-7.61298704116733,
6.99972967223882));
#12259=CARTESIAN_POINT('Ctrl Pts',(-13.2372839439424,-8.32932353917012,
6.88858852470981));
#12260=CARTESIAN_POINT('Ctrl Pts',(-12.64038931445,-10.5749548961775,6.77744737718078));
#12261=CARTESIAN_POINT('Ctrl Pts',(-14.2033970972384,-12.2942830560246,
6.66630622965177));
#12262=CARTESIAN_POINT('Ctrl Pts',(-16.4955795141811,-11.9135215156732,
6.55516508212274));
#12263=CARTESIAN_POINT('Ctrl Pts',(-17.4187697235728,-9.78119478057994,
6.44402393459372));
#12264=CARTESIAN_POINT('Ctrl Pts',(-16.1279126463626,-7.84915537048691,
6.3328827870647));
#12265=CARTESIAN_POINT('Ctrl Pts',(-13.8046094981315,-7.88591323323186,
6.22174163953568));
#12266=CARTESIAN_POINT('Ctrl Pts',(-12.5755192591945,-9.85782298675155,
6.11060049200667));
#12267=CARTESIAN_POINT('Ctrl Pts',(-13.5657029889766,-11.9598757266924,
5.99945934447763));
#12268=CARTESIAN_POINT('Ctrl Pts',(-15.8687854179254,-12.2679358305796,
5.88831819694863));
#12269=CARTESIAN_POINT('Ctrl Pts',(-17.3766160640088,-10.5000170785009,
5.7771770494196));
#12270=CARTESIAN_POINT('Ctrl Pts',(-16.7089863056128,-8.27440249298907,
5.66603590189059));
#12271=CARTESIAN_POINT('Ctrl Pts',(-14.4770180600175,-7.62833162617035,
5.55489475436157));
#12272=CARTESIAN_POINT('Ctrl Pts',(-12.7237668001956,-9.15319223134576,
5.44375360683254));
#12273=CARTESIAN_POINT('Ctrl Pts',(-13.0540894216228,-11.4531871843689,
5.33261245930352));
#12274=CARTESIAN_POINT('Ctrl Pts',(-15.1656216518599,-12.4229920439975,
5.22147131177451));
#12275=CARTESIAN_POINT('Ctrl Pts',(-17.1255503707361,-11.1748857803501,
5.11033016424548));
#12276=CARTESIAN_POINT('Ctrl Pts',(-17.1398343152041,-8.85133552402972,
4.99918901671647));
#12277=CARTESIAN_POINT('Ctrl Pts',(-15.1953985278237,-7.57922731532253,
4.88804786918744));
#12278=CARTESIAN_POINT('Ctrl Pts',(-13.0721026532078,-8.52299871511589,
4.77690672165843));
#12279=CARTESIAN_POINT('Ctrl Pts',(-12.7135277889139,-10.818758696566,4.6657655741294));
#12280=CARTESIAN_POINT('Ctrl Pts',(-14.4478991890863,-12.3650593375113,
4.55462442660038));
#12281=CARTESIAN_POINT('Ctrl Pts',(-16.6876418438301,-11.7464781654166,
4.44348327907137));
#12282=CARTESIAN_POINT('Ctrl Pts',(-17.3825838770138,-9.52923992914208,
4.33234213154235));
#12283=CARTESIAN_POINT('Ctrl Pts',(-15.8966028265696,-7.74291684984371,
4.22120098401332));
#12284=CARTESIAN_POINT('Ctrl Pts',(-13.5899069966017,-8.02263845058788,
4.11005983648432));
#12285=CARTESIAN_POINT('Ctrl Pts',(-12.5739545527748,-10.1123586370691,
3.99891868895528));
#12286=CARTESIAN_POINT('Ctrl Pts',(-13.7787081956621,-12.0992301693682,
3.88777754142627));
#12287=CARTESIAN_POINT('Ctrl Pts',(-16.1013840714784,-12.1645493993947,
3.77663639389725));
#12288=CARTESIAN_POINT('Ctrl Pts',(-17.4158965123757,-10.248525686433,3.66549524636823));
#12289=CARTESIAN_POINT('Ctrl Pts',(-16.5189928002739,-8.10501138577344,
3.55435409883921));
#12290=CARTESIAN_POINT('Ctrl Pts',(-14.2316631334124,-7.69609474266784,
3.44321295131019));
#12291=CARTESIAN_POINT('Ctrl Pts',(-12.647638657407,-9.39608188535426,3.33207180378117));
#12292=CARTESIAN_POINT('Ctrl Pts',(-13.2168727518909,-11.6488717938068,
3.22093065625215));
#12293=CARTESIAN_POINT('Ctrl Pts',(-15.4183110319232,-12.3923496516694,
3.10978950872312));
#12294=CARTESIAN_POINT('Ctrl Pts',(-17.2368439315762,-10.9459652219235,
2.99864836119411));
#12295=CARTESIAN_POINT('Ctrl Pts',(-17.0078583317483,-8.63368162744371,
2.88750721366509));
#12296=CARTESIAN_POINT('Ctrl Pts',(-14.9409585972601,-7.57207185286643,
2.77636606613607));
#12297=CARTESIAN_POINT('Ctrl Pts',(-12.9281030287572,-8.73289151373681,
2.66522491860704));
#12298=CARTESIAN_POINT('Ctrl Pts',(-12.8117800332785,-11.0535721874087,
2.55408377107803));
#12299=CARTESIAN_POINT('Ctrl Pts',(-14.6984670829124,-12.4098545333209,
2.442942623549));
#12300=CARTESIAN_POINT('Ctrl Pts',(-16.8611654422835,-11.5602513173828,
2.33180147601999));
#12301=CARTESIAN_POINT('Ctrl Pts',(-17.3202265408315,-9.28245572666732,
2.22066032849097));
#12302=CARTESIAN_POINT('Ctrl Pts',(-15.6554439913718,-7.66147180407228,
2.10951918096195));
#12303=CARTESIAN_POINT('Ctrl Pts',(-13.3906939345767,-8.18108411896286,
1.99837803343293));
#12304=CARTESIAN_POINT('Ctrl Pts',(-12.5990390076834,-10.3656601528754,
1.88723688590391));
#12305=CARTESIAN_POINT('Ctrl Pts',(-14.0051288824869,-12.2155252739355,
1.77609573837489));
#12306=CARTESIAN_POINT('Ctrl Pts',(-16.3218843807385,-12.0373862789351,
1.66495459084587));
#12307=CARTESIAN_POINT('Ctrl Pts',(-17.428639303623,-9.99430418754786,1.55381344331685));
#12308=CARTESIAN_POINT('Ctrl Pts',(-16.3123135839388,-7.95643629520889,
1.44267229578783));
#12309=CARTESIAN_POINT('Ctrl Pts',(-13.9947483624482,-7.78916489875036,
1.33153114825881));
#12310=CARTESIAN_POINT('Ctrl Pts',(-12.5973498364434,-9.64560634071132,
1.22039000072979));
#12311=CARTESIAN_POINT('Ctrl Pts',(-13.3992440433914,-11.826442250177,1.10924885320077));
#12312=CARTESIAN_POINT('Ctrl Pts',(-15.6664035468934,-12.3354318728424,
0.998107705671752));
#12313=CARTESIAN_POINT('Ctrl Pts',(-17.32357021704,-10.7066464303587,0.88696655814273));
#12314=CARTESIAN_POINT('Ctrl Pts',(-16.8538197307884,-8.43105010031595,
0.775825410613713));
#12315=CARTESIAN_POINT('Ctrl Pts',(-14.687180849695,-7.59155940883828,0.664684263084691));
#12316=CARTESIAN_POINT('Ctrl Pts',(-12.8068360000695,-8.95675512341312,
0.553543115555673));
#12317=CARTESIAN_POINT('Ctrl Pts',(-12.9341202906761,-11.2767116091318,
0.442401968026652));
#12318=CARTESIAN_POINT('Ctrl Pts',(-14.9522479049698,-12.4283740802081,
0.331260820497633));
#12319=CARTESIAN_POINT('Ctrl Pts',(-17.0144374426264,-11.3565061871398,
0.220119672968612));
#12320=CARTESIAN_POINT('Ctrl Pts',(-17.2320075214997,-9.04429062969129,
0.108978525439591));
#12321=CARTESIAN_POINT('Ctrl Pts',(-15.407826937649,-7.60427002768573,-0.00216262208942734));
#12322=CARTESIAN_POINT('Ctrl Pts',(-13.2075718205704,-8.36246714664345,
-0.113303769618448));
#12323=CARTESIAN_POINT('Ctrl Pts',(-12.839200671623,-9.85926548464067,-0.187397867971127));
#12324=CARTESIAN_POINT('Ctrl Pts',(-13.0122087991468,-10.5202727210901,
-0.224444917147467));
#12325=CARTESIAN_POINT('Ctrl Pts',(-15.4967348970877,-11.8599788000028,
8.07481497238249));
#12326=CARTESIAN_POINT('Ctrl Pts',(-16.1152402239634,-11.6947977883195,
8.03776792320615));
#12327=CARTESIAN_POINT('Ctrl Pts',(-17.163797181446,-10.7016300569196,7.96367382485347));
#12328=CARTESIAN_POINT('Ctrl Pts',(-16.7624646904471,-8.55842281702485,
7.85253267732444));
#12329=CARTESIAN_POINT('Ctrl Pts',(-14.7448372528894,-7.73946748106473,
7.74139152979544));
#12330=CARTESIAN_POINT('Ctrl Pts',(-12.9622917582753,-8.98740724711157,
7.6302503822664));
#12331=CARTESIAN_POINT('Ctrl Pts',(-13.0442050684083,-11.1634133319412,
7.51910923473739));
#12332=CARTESIAN_POINT('Ctrl Pts',(-14.9167771789417,-12.2738697274138,
7.40796808720837));
#12333=CARTESIAN_POINT('Ctrl Pts',(-16.8653210847252,-11.3032287952692,
7.29682693967936));
#12334=CARTESIAN_POINT('Ctrl Pts',(-17.1065306557073,-9.13950220880304,
7.18568579215032));
#12335=CARTESIAN_POINT('Ctrl Pts',(-15.4194502259573,-7.7635246228271,7.07454464462132));
#12336=CARTESIAN_POINT('Ctrl Pts',(-13.348450082044,-8.43468517670065,6.96340349709229));
#12337=CARTESIAN_POINT('Ctrl Pts',(-12.7891987647493,-10.5386952188625,
6.85226234956327));
#12338=CARTESIAN_POINT('Ctrl Pts',(-14.253635062676,-12.1495935093596,6.74112120203425));
#12339=CARTESIAN_POINT('Ctrl Pts',(-16.4012604102937,-11.79284479276,6.62998005450523));
#12340=CARTESIAN_POINT('Ctrl Pts',(-17.2662293934371,-9.79499378760424,
6.51883890697621));
#12341=CARTESIAN_POINT('Ctrl Pts',(-16.0567805473605,-7.98479893616371,
6.4076977594472));
#12342=CARTESIAN_POINT('Ctrl Pts',(-13.8799971053183,-8.01923865491027,
6.29655661191817));
#12343=CARTESIAN_POINT('Ctrl Pts',(-12.72841975609,-9.86678941639023,6.18541546438916));
#12344=CARTESIAN_POINT('Ctrl Pts',(-13.6561572961568,-11.8362756636269,
6.07427431686014));
#12345=CARTESIAN_POINT('Ctrl Pts',(-15.8139952437406,-12.1249078784139,
5.9631331693311));
#12346=CARTESIAN_POINT('Ctrl Pts',(-17.2267341651754,-10.4684833737895,
5.85199202180211));
#12347=CARTESIAN_POINT('Ctrl Pts',(-16.6012086479404,-8.3832277403185,5.74085087427306));
#12348=CARTESIAN_POINT('Ctrl Pts',(-14.5100000495813,-7.77790149765939,
5.62970972674407));
#12349=CARTESIAN_POINT('Ctrl Pts',(-12.8673180280698,-9.20659637946829,
5.51856857921502));
#12350=CARTESIAN_POINT('Ctrl Pts',(-13.1768087690445,-11.361541563584,5.40742743168602));
#12351=CARTESIAN_POINT('Ctrl Pts',(-15.1551766801017,-12.2701854321462,
5.29628628415699));
#12352=CARTESIAN_POINT('Ctrl Pts',(-16.9915019939467,-11.1007913086607,
5.18514513662797));
#12353=CARTESIAN_POINT('Ctrl Pts',(-17.0048851178101,-8.923776342464,5.07400398909896));
#12354=CARTESIAN_POINT('Ctrl Pts',(-15.1830756697807,-7.73189396271163,
4.96286284156994));
#12355=CARTESIAN_POINT('Ctrl Pts',(-13.1936859915807,-8.61614617822962,
4.85172169404091));
#12356=CARTESIAN_POINT('Ctrl Pts',(-12.8577247426487,-10.7671234703357,
4.7405805465119));
#12357=CARTESIAN_POINT('Ctrl Pts',(-14.4827175676795,-12.215906266585,4.62943939898287));
#12358=CARTESIAN_POINT('Ctrl Pts',(-16.5812102800893,-11.6363360740339,
4.51829825145386));
#12359=CARTESIAN_POINT('Ctrl Pts',(-17.2323256165297,-9.55892853319708,
4.40715710392483));
#12360=CARTESIAN_POINT('Ctrl Pts',(-15.8400583404068,-7.88526037494785,
4.29601595639582));
#12361=CARTESIAN_POINT('Ctrl Pts',(-13.6788348718617,-8.1473412615274,4.1848748088668));
#12362=CARTESIAN_POINT('Ctrl Pts',(-12.7269537282801,-10.1052727109369,
4.07373366133778));
#12363=CARTESIAN_POINT('Ctrl Pts',(-13.8557292751018,-11.9668416827977,
3.96259251380875));
#12364=CARTESIAN_POINT('Ctrl Pts',(-16.0319250038243,-12.0280415389064,
3.85145136627974));
#12365=CARTESIAN_POINT('Ctrl Pts',(-17.2635373820377,-10.2328523505688,
3.74031021875071));
#12366=CARTESIAN_POINT('Ctrl Pts',(-16.4231971315216,-8.22451932652546,
3.6291690712217));
#12367=CARTESIAN_POINT('Ctrl Pts',(-14.2801184940623,-7.84139111591484,
3.51802792369268));
#12368=CARTESIAN_POINT('Ctrl Pts',(-12.795990926042,-9.43416813543636,3.40688677616365));
#12369=CARTESIAN_POINT('Ctrl Pts',(-13.3293261270302,-11.5448852731689,
3.29574562863464));
#12370=CARTESIAN_POINT('Ctrl Pts',(-15.391930139899,-12.2414755101134,3.18460448110562));
#12371=CARTESIAN_POINT('Ctrl Pts',(-17.0957767979589,-10.8863076836954,
3.0734633335766));
#12372=CARTESIAN_POINT('Ctrl Pts',(-16.8812322334449,-8.71984884443381,
2.96232218604758));
#12373=CARTESIAN_POINT('Ctrl Pts',(-14.9446820583973,-7.72518976132214,
2.85118103851856));
#12374=CARTESIAN_POINT('Ctrl Pts',(-13.0587677402097,-8.81280203391929,
2.74003989098954));
#12375=CARTESIAN_POINT('Ctrl Pts',(-12.9497806841384,-10.9871283884299,
2.62889874346052));
#12376=CARTESIAN_POINT('Ctrl Pts',(-14.7174833333107,-12.2578764419345,
2.5177575959315));
#12377=CARTESIAN_POINT('Ctrl Pts',(-16.7437905685052,-11.4618536697156,
2.40661644840248));
#12378=CARTESIAN_POINT('Ctrl Pts',(-17.1739008616738,-9.32770783945607,
2.29547530087346));
#12379=CARTESIAN_POINT('Ctrl Pts',(-15.6141082487193,-7.80895168178116,
2.18433415334444));
#12380=CARTESIAN_POINT('Ctrl Pts',(-13.4921852324529,-8.2957945133747,2.07319300581542));
#12381=CARTESIAN_POINT('Ctrl Pts',(-12.7504562256358,-10.3425997019803,
1.9620518582864));
#12382=CARTESIAN_POINT('Ctrl Pts',(-14.0678706835062,-12.0758026069051,
1.85091071075738));
#12383=CARTESIAN_POINT('Ctrl Pts',(-16.2385194047865,-11.9088979931037,
1.73976956322836));
#12384=CARTESIAN_POINT('Ctrl Pts',(-17.2754765459017,-9.99466339541431,
1.62862841569934));
#12385=CARTESIAN_POINT('Ctrl Pts',(-16.2295521927304,-8.08531416197898,
1.51748726817032));
#12386=CARTESIAN_POINT('Ctrl Pts',(-14.0581448136139,-7.92859177884296,
1.4063461206413));
#12387=CARTESIAN_POINT('Ctrl Pts',(-12.7488735824113,-9.66795626731204,
1.29520497311228));
#12388=CARTESIAN_POINT('Ctrl Pts',(-13.5001961264723,-11.7112572033738,
1.18406382558326));
#12389=CARTESIAN_POINT('Ctrl Pts',(-15.6243766370739,-12.1881472655394,
1.07292267805424));
#12390=CARTESIAN_POINT('Ctrl Pts',(-17.1770336680885,-10.6620815928193,
0.961781530525219));
#12391=CARTESIAN_POINT('Ctrl Pts',(-16.7369081161809,-8.52999632629676,
0.850640382996202));
#12392=CARTESIAN_POINT('Ctrl Pts',(-14.7069088692726,-7.74344832960141,
0.73949923546718));
#12393=CARTESIAN_POINT('Ctrl Pts',(-12.9451484476459,-9.02254762789837,
0.628358087938162));
#12394=CARTESIAN_POINT('Ctrl Pts',(-13.0644055219694,-11.1961954655539,
0.517216940409141));
#12395=CARTESIAN_POINT('Ctrl Pts',(-14.9552594030341,-12.2752280488692,
0.406075792880122));
#12396=CARTESIAN_POINT('Ctrl Pts',(-16.8873964310158,-11.270957778128,0.294934645351101));
#12397=CARTESIAN_POINT('Ctrl Pts',(-17.0912453973186,-9.10456268512506,
0.183793497822081));
#12398=CARTESIAN_POINT('Ctrl Pts',(-15.3821072277069,-7.75535735002619,
0.0726523502930616));
#12399=CARTESIAN_POINT('Ctrl Pts',(-13.3206117613179,-8.46573857410703,
-0.038488797235959));
#12400=CARTESIAN_POINT('Ctrl Pts',(-12.9754720329252,-9.86814094278172,
-0.112582895588638));
#12401=CARTESIAN_POINT('Ctrl Pts',(-13.1375693587171,-10.4874615891075,
-0.149629944764978));
#12402=CARTESIAN_POINT('Ctrl Pts',(-15.4632995769868,-11.7347832743338,
8.14962994476498));
#12403=CARTESIAN_POINT('Ctrl Pts',(-16.0401731930456,-11.5807206278643,
8.11258289558864));
#12404=CARTESIAN_POINT('Ctrl Pts',(-17.01815158292,-10.6544032047635,8.03848879723596));
#12405=CARTESIAN_POINT('Ctrl Pts',(-16.6438328579804,-8.65545565052525,
7.92734764970694));
#12406=CARTESIAN_POINT('Ctrl Pts',(-14.7620123057747,-7.89162435349761,
7.81620650217792));
#12407=CARTESIAN_POINT('Ctrl Pts',(-13.099450286363,-9.05556505728998,7.7050653546489));
#12408=CARTESIAN_POINT('Ctrl Pts',(-13.1758499960607,-11.085103759992,7.59392420711988));
#12409=CARTESIAN_POINT('Ctrl Pts',(-14.9223789228056,-12.1208151249496,
7.48278305959086));
#12410=CARTESIAN_POINT('Ctrl Pts',(-16.7397659688587,-11.2155082179753,
7.37164191206185));
#12411=CARTESIAN_POINT('Ctrl Pts',(-16.9647396778862,-9.19742247827372,
7.26050076453281));
#12412=CARTESIAN_POINT('Ctrl Pts',(-15.3912169517229,-7.91406220448686,
7.1493596170038));
#12413=CARTESIAN_POINT('Ctrl Pts',(-13.4596162201455,-8.54004681423119,
7.03821846947478));
#12414=CARTESIAN_POINT('Ctrl Pts',(-12.9380082150486,-10.5024355415475,
6.92707732194577));
#12415=CARTESIAN_POINT('Ctrl Pts',(-14.3038730281136,-12.0049039626946,
6.81593617441673));
#12416=CARTESIAN_POINT('Ctrl Pts',(-16.3069413064063,-11.6721680698467,
6.70479502688773));
#12417=CARTESIAN_POINT('Ctrl Pts',(-17.1136890633015,-9.80879279462856,
6.59365387935869));
#12418=CARTESIAN_POINT('Ctrl Pts',(-15.9856484483585,-8.1204425018405,6.48251273182969));
#12419=CARTESIAN_POINT('Ctrl Pts',(-13.9553847125051,-8.15256407658869,
6.37137158430066));
#12420=CARTESIAN_POINT('Ctrl Pts',(-12.8813202529855,-9.87575584602892,
6.26023043677165));
#12421=CARTESIAN_POINT('Ctrl Pts',(-13.746611603337,-11.7126756005614,6.14908928924262));
#12422=CARTESIAN_POINT('Ctrl Pts',(-15.7592050695559,-11.9818799262481,
6.0379481417136));
#12423=CARTESIAN_POINT('Ctrl Pts',(-17.0768522663421,-10.4369496690781,
5.92680699418459));
#12424=CARTESIAN_POINT('Ctrl Pts',(-16.493430990268,-8.49205298764794,5.81566584665555));
#12425=CARTESIAN_POINT('Ctrl Pts',(-14.542982039145,-7.92747136914842,5.70452469912656));
#12426=CARTESIAN_POINT('Ctrl Pts',(-13.0108692559441,-9.26000052759082,
5.59338355159751));
#12427=CARTESIAN_POINT('Ctrl Pts',(-13.2995281164661,-11.2698959427991,
5.48224240406851));
#12428=CARTESIAN_POINT('Ctrl Pts',(-15.1447317083435,-12.117378820295,5.37110125653948));
#12429=CARTESIAN_POINT('Ctrl Pts',(-16.8574536171574,-11.0266968369714,
5.25996010901046));
#12430=CARTESIAN_POINT('Ctrl Pts',(-16.8699359204162,-8.99621716089825,
5.14881896148145));
#12431=CARTESIAN_POINT('Ctrl Pts',(-15.1707528117377,-7.88456061010077,
5.03767781395242));
#12432=CARTESIAN_POINT('Ctrl Pts',(-13.3152693299537,-8.7092936413433,4.9265366664234));
#12433=CARTESIAN_POINT('Ctrl Pts',(-13.0019216963835,-10.7154882441055,
4.81539551889438));
#12434=CARTESIAN_POINT('Ctrl Pts',(-14.5175359462726,-12.0667531956587,
4.70425437136536));
#12435=CARTESIAN_POINT('Ctrl Pts',(-16.4747787163486,-11.5261939826513,
4.59311322383635));
#12436=CARTESIAN_POINT('Ctrl Pts',(-17.0820673560456,-9.58861713725206,
4.48197207630732));
#12437=CARTESIAN_POINT('Ctrl Pts',(-15.7835138542441,-8.02760390005202,
4.37083092877831));
#12438=CARTESIAN_POINT('Ctrl Pts',(-13.7677627471216,-8.27204407246692,
4.25968978124928));
#12439=CARTESIAN_POINT('Ctrl Pts',(-12.8799529037855,-10.0981867848047,
4.14854863372027));
#12440=CARTESIAN_POINT('Ctrl Pts',(-13.9327503545415,-11.8344531962273,
4.03740748619124));
#12441=CARTESIAN_POINT('Ctrl Pts',(-15.9624659361701,-11.8915336784182,
3.92626633866223));
#12442=CARTESIAN_POINT('Ctrl Pts',(-17.1111782516997,-10.2171790147046,
3.81512519113321));
#12443=CARTESIAN_POINT('Ctrl Pts',(-16.3274014627693,-8.34402726727746,
3.70398404360418));
#12444=CARTESIAN_POINT('Ctrl Pts',(-14.3285738547121,-7.98668748916186,
3.59284289607517));
#12445=CARTESIAN_POINT('Ctrl Pts',(-12.9443431946769,-9.47225438551843,
3.48170174854614));
#12446=CARTESIAN_POINT('Ctrl Pts',(-13.4417795021695,-11.440898752531,3.37056060101713));
#12447=CARTESIAN_POINT('Ctrl Pts',(-15.3655492478748,-12.0906013685574,
3.2594194534881));
#12448=CARTESIAN_POINT('Ctrl Pts',(-16.9547096643416,-10.8266501454673,
3.14827830595909));
#12449=CARTESIAN_POINT('Ctrl Pts',(-16.7546061351414,-8.80601606142392,
3.03713715843006));
#12450=CARTESIAN_POINT('Ctrl Pts',(-14.9484055195346,-7.87830766977787,
2.92599601090105));
#12451=CARTESIAN_POINT('Ctrl Pts',(-13.1894324516621,-8.89271255410176,
2.81485486337202));
#12452=CARTESIAN_POINT('Ctrl Pts',(-13.0877813349982,-10.9206845894511,
2.70371371584301));
#12453=CARTESIAN_POINT('Ctrl Pts',(-14.736499583709,-12.1058983505481,2.59257256831398));
#12454=CARTESIAN_POINT('Ctrl Pts',(-16.6264156947269,-11.3634560220484,
2.48143142078497));
#12455=CARTESIAN_POINT('Ctrl Pts',(-17.027575182516,-9.37295995224483,2.37029027325595));
#12456=CARTESIAN_POINT('Ctrl Pts',(-15.5727725060668,-7.95643155949003,
2.25914912572693));
#12457=CARTESIAN_POINT('Ctrl Pts',(-13.5936765303291,-8.41050490778654,
2.14800797819791));
#12458=CARTESIAN_POINT('Ctrl Pts',(-12.9018734435882,-10.3195392510852,
2.03686683066889));
#12459=CARTESIAN_POINT('Ctrl Pts',(-14.1306124845255,-11.9360799398746,
1.92572568313987));
#12460=CARTESIAN_POINT('Ctrl Pts',(-16.1551544288345,-11.7804097072723,
1.81458453561085));
#12461=CARTESIAN_POINT('Ctrl Pts',(-17.1223137881804,-9.99502260328078,
1.70344338808183));
#12462=CARTESIAN_POINT('Ctrl Pts',(-16.1467908015221,-8.21419202874906,
1.59230224055281));
#12463=CARTESIAN_POINT('Ctrl Pts',(-14.1215412647796,-8.06801865893557,
1.48116109302379));
#12464=CARTESIAN_POINT('Ctrl Pts',(-12.9003973283792,-9.69030619391275,
1.37001994549477));
#12465=CARTESIAN_POINT('Ctrl Pts',(-13.6011482095532,-11.5960721565707,
1.25887879796575));
#12466=CARTESIAN_POINT('Ctrl Pts',(-15.5823497272544,-12.0408626582364,
1.14773765043673));
#12467=CARTESIAN_POINT('Ctrl Pts',(-17.030497119137,-10.61751675528,1.03659650290771));
#12468=CARTESIAN_POINT('Ctrl Pts',(-16.6199965015735,-8.62894255227754,
0.92545535537869));
#12469=CARTESIAN_POINT('Ctrl Pts',(-14.7266368888501,-7.89533725036455,
0.814314207849669));
#12470=CARTESIAN_POINT('Ctrl Pts',(-13.0834608952223,-9.0883401323836,0.703173060320652));
#12471=CARTESIAN_POINT('Ctrl Pts',(-13.1946907532627,-11.115679321976,0.59203191279163));
#12472=CARTESIAN_POINT('Ctrl Pts',(-14.9582709010984,-12.1220820175303,
0.480890765262611));
#12473=CARTESIAN_POINT('Ctrl Pts',(-16.7603554194051,-11.1854093691163,
0.369749617733591));
#12474=CARTESIAN_POINT('Ctrl Pts',(-16.9504832731376,-9.1648347405588,0.258608470204569));
#12475=CARTESIAN_POINT('Ctrl Pts',(-15.3563875177647,-7.90644467236664,
0.147467322675551));
#12476=CARTESIAN_POINT('Ctrl Pts',(-13.4336517020655,-8.56901000157061,
0.0363261751465299));
#12477=CARTESIAN_POINT('Ctrl Pts',(-13.1117433942273,-9.87701640092276,
-0.0377679232061492));
#12478=CARTESIAN_POINT('Ctrl Pts',(-13.2629299182875,-10.4546504571249,
-0.0748149723824891));
#12479=CARTESIAN_POINT('Ctrl Pts',(-15.4298642568859,-11.6095877486648,
8.22444491714747));
#12480=CARTESIAN_POINT('Ctrl Pts',(-15.9651061621278,-11.4666434674091,
8.18739786797113));
#12481=CARTESIAN_POINT('Ctrl Pts',(-16.872505984394,-10.6071763526074,8.11330376961845));
#12482=CARTESIAN_POINT('Ctrl Pts',(-16.5252010255137,-8.75248848402567,
8.00216262208943));
#12483=CARTESIAN_POINT('Ctrl Pts',(-14.7791873586601,-8.04378122593049,
7.89102147456041));
#12484=CARTESIAN_POINT('Ctrl Pts',(-13.2366088144507,-9.12372286746838,
7.7798803270314));
#12485=CARTESIAN_POINT('Ctrl Pts',(-13.3074949237131,-11.0067941880429,
7.66873917950236));
#12486=CARTESIAN_POINT('Ctrl Pts',(-14.9279806666696,-11.9677605224854,
7.55759803197335));
#12487=CARTESIAN_POINT('Ctrl Pts',(-16.6142108529922,-11.1277876406814,
7.44645688444433));
#12488=CARTESIAN_POINT('Ctrl Pts',(-16.822948700065,-9.25534274774437,7.3353157369153));
#12489=CARTESIAN_POINT('Ctrl Pts',(-15.3629836774885,-8.06459978614663,
7.22417458938629));
#12490=CARTESIAN_POINT('Ctrl Pts',(-13.570782358247,-8.64540845176172,7.11303344185727));
#12491=CARTESIAN_POINT('Ctrl Pts',(-13.0868176653479,-10.4661758642325,
7.00189229432825));
#12492=CARTESIAN_POINT('Ctrl Pts',(-14.3541109935512,-11.8602144160296,
6.89075114679923));
#12493=CARTESIAN_POINT('Ctrl Pts',(-16.2126222025189,-11.5514913469335,
6.77960999927021));
#12494=CARTESIAN_POINT('Ctrl Pts',(-16.9611487331658,-9.82259180165284,
6.66846885174119));
#12495=CARTESIAN_POINT('Ctrl Pts',(-15.9145163493564,-8.25608606751732,
6.55732770421217));
#12496=CARTESIAN_POINT('Ctrl Pts',(-14.0307723196919,-8.28588949826707,
6.44618655668315));
#12497=CARTESIAN_POINT('Ctrl Pts',(-13.034220749881,-9.88472227566764,6.33504540915413));
#12498=CARTESIAN_POINT('Ctrl Pts',(-13.8370659105171,-11.5890755374958,
6.22390426162511));
#12499=CARTESIAN_POINT('Ctrl Pts',(-15.7044148953711,-11.8388519740824,
6.11276311409609));
#12500=CARTESIAN_POINT('Ctrl Pts',(-16.9269703675087,-10.4054159643667,
6.00162196656707));
#12501=CARTESIAN_POINT('Ctrl Pts',(-16.3856533325956,-8.60087823497738,
5.89048081903805));
#12502=CARTESIAN_POINT('Ctrl Pts',(-14.5759640287087,-8.07704124063746,
5.77933967150903));
#12503=CARTESIAN_POINT('Ctrl Pts',(-13.1544204838184,-9.31340467571335,
5.66819852398002));
#12504=CARTESIAN_POINT('Ctrl Pts',(-13.4222474638878,-11.1782503220142,
5.55705737645098));
#12505=CARTESIAN_POINT('Ctrl Pts',(-15.1342867365853,-11.9645722084437,
5.44591622892198));
#12506=CARTESIAN_POINT('Ctrl Pts',(-16.723405240368,-10.952602365282,5.33477508139295));
#12507=CARTESIAN_POINT('Ctrl Pts',(-16.7349867230223,-9.06865797933251,
5.22363393386394));
#12508=CARTESIAN_POINT('Ctrl Pts',(-15.1584299536947,-8.0372272574899,5.11249278633491));
#12509=CARTESIAN_POINT('Ctrl Pts',(-13.4368526683266,-8.80244110445702,
5.00135163880589));
#12510=CARTESIAN_POINT('Ctrl Pts',(-13.1461186501183,-10.6638530178752,
4.89021049127687));
#12511=CARTESIAN_POINT('Ctrl Pts',(-14.5523543248657,-11.9176001247324,
4.77906934374785));
#12512=CARTESIAN_POINT('Ctrl Pts',(-16.3683471526078,-11.4160518912686,
4.66792819621883));
#12513=CARTESIAN_POINT('Ctrl Pts',(-16.9318090955615,-9.61830574130706,
4.55678704868981));
#12514=CARTESIAN_POINT('Ctrl Pts',(-15.7269693680813,-8.16994742515617,
4.44564590116079));
#12515=CARTESIAN_POINT('Ctrl Pts',(-13.8566906223815,-8.39674688340643,
4.33450475363178));
#12516=CARTESIAN_POINT('Ctrl Pts',(-13.0329520792908,-10.0911008586724,
4.22336360610275));
#12517=CARTESIAN_POINT('Ctrl Pts',(-14.0097714339813,-11.7020647096568,
4.11222245857374));
#12518=CARTESIAN_POINT('Ctrl Pts',(-15.8930068685159,-11.7550258179299,
4.00108131104471));
#12519=CARTESIAN_POINT('Ctrl Pts',(-16.9588191213617,-10.2015056788404,
3.88994016351569));
#12520=CARTESIAN_POINT('Ctrl Pts',(-16.2316057940169,-8.46353520802948,
3.77879901598668));
#12521=CARTESIAN_POINT('Ctrl Pts',(-14.377029215362,-8.13198386240885,3.66765786845765));
#12522=CARTESIAN_POINT('Ctrl Pts',(-13.0926954633119,-9.51034063560054,
3.55651672092863));
#12523=CARTESIAN_POINT('Ctrl Pts',(-13.5542328773088,-11.336912231893,3.44537557339961));
#12524=CARTESIAN_POINT('Ctrl Pts',(-15.3391683558506,-11.9397272270015,
3.3342344258706));
#12525=CARTESIAN_POINT('Ctrl Pts',(-16.8136425307244,-10.7669926072391,
3.22309327834158));
#12526=CARTESIAN_POINT('Ctrl Pts',(-16.627980036838,-8.89218327841403,3.11195213081255));
#12527=CARTESIAN_POINT('Ctrl Pts',(-14.9521289806718,-8.03142557823359,
3.00081098328354));
#12528=CARTESIAN_POINT('Ctrl Pts',(-13.3200971631145,-8.97262307428424,
2.88966983575451));
#12529=CARTESIAN_POINT('Ctrl Pts',(-13.2257819858581,-10.8542407904722,
2.7785286882255));
#12530=CARTESIAN_POINT('Ctrl Pts',(-14.7555158341074,-11.9539202591618,
2.66738754069647));
#12531=CARTESIAN_POINT('Ctrl Pts',(-16.5090408209486,-11.2650583743812,
2.55624639316746));
#12532=CARTESIAN_POINT('Ctrl Pts',(-16.8812495033582,-9.41821206503357,
2.44510524563843));
#12533=CARTESIAN_POINT('Ctrl Pts',(-15.5314367634142,-8.1039114371989,2.33396409810942));
#12534=CARTESIAN_POINT('Ctrl Pts',(-13.6951678282053,-8.52521530219838,
2.2228229505804));
#12535=CARTESIAN_POINT('Ctrl Pts',(-13.0532906615406,-10.29647880019,2.11168180305138));
#12536=CARTESIAN_POINT('Ctrl Pts',(-14.1933542855448,-11.7963572728442,
2.00054065552236));
#12537=CARTESIAN_POINT('Ctrl Pts',(-16.0717894528825,-11.651921421441,1.88939950799334));
#12538=CARTESIAN_POINT('Ctrl Pts',(-16.9691510304591,-9.99538181114722,
1.77825836046432));
#12539=CARTESIAN_POINT('Ctrl Pts',(-16.0640294103137,-8.34306989551916,
1.6671172129353));
#12540=CARTESIAN_POINT('Ctrl Pts',(-14.1849377159453,-8.20744553902816,
1.55597606540628));
#12541=CARTESIAN_POINT('Ctrl Pts',(-13.0519210743471,-9.71265612051347,
1.44483491787726));
#12542=CARTESIAN_POINT('Ctrl Pts',(-13.7021002926342,-11.4808871097675,
1.33369377034824));
#12543=CARTESIAN_POINT('Ctrl Pts',(-15.5403228174349,-11.8935780509334,
1.22255262281922));
#12544=CARTESIAN_POINT('Ctrl Pts',(-16.8839605701855,-10.5729519177407,
1.1114114752902));
#12545=CARTESIAN_POINT('Ctrl Pts',(-16.503084886966,-8.72788877825835,1.00027032776118));
#12546=CARTESIAN_POINT('Ctrl Pts',(-14.7463649084277,-8.04722617112768,
0.889129180232157));
#12547=CARTESIAN_POINT('Ctrl Pts',(-13.2217733427987,-9.15413263686884,
0.777988032703141));
#12548=CARTESIAN_POINT('Ctrl Pts',(-13.324975984556,-11.0351631783981,0.666846885174119));
#12549=CARTESIAN_POINT('Ctrl Pts',(-14.9612823991627,-11.9689359861914,
0.5557057376451));
#12550=CARTESIAN_POINT('Ctrl Pts',(-16.6333144077944,-11.0998609601046,
0.444564590116079));
#12551=CARTESIAN_POINT('Ctrl Pts',(-16.8097211489565,-9.22510679599255,
0.333423442587059));
#12552=CARTESIAN_POINT('Ctrl Pts',(-15.3306678078225,-8.0575319947071,0.22228229505804));
#12553=CARTESIAN_POINT('Ctrl Pts',(-13.5466916428131,-8.67228142903419,
0.111141147529019));
#12554=CARTESIAN_POINT('Ctrl Pts',(-13.2480147555294,-9.88589185906381,
0.0370470491763399));
#12555=CARTESIAN_POINT('Ctrl Pts',(-13.3882904778579,-10.4218393251423,
0.));
#12556=CARTESIAN_POINT('Ctrl Pts',(-13.3882904778579,-10.4218393251423,
0.));
#12557=CARTESIAN_POINT('Ctrl Pts',(-13.3657944025764,-10.364062743702,-3.7859623319602E-17));
#12558=CARTESIAN_POINT('Ctrl Pts',(-13.3468720776219,-10.3051562840246,
1.43829901930131E-15));
#12559=CARTESIAN_POINT('Ctrl Pts',(-13.3313727935116,-10.2454301582812,
1.2490009027033E-15));
#12560=CARTESIAN_POINT('Ctrl Pts',(-13.3148521018426,-10.1817680626023,
1.04722798238191E-15));
#12561=CARTESIAN_POINT('Ctrl Pts',(-13.3022199241254,-10.1171741832588,
-2.07892182731082E-15));
#12562=CARTESIAN_POINT('Ctrl Pts',(-13.2933434453493,-10.0519874094327,
-1.55431223447522E-15));
#12563=CARTESIAN_POINT('Ctrl Pts',(-13.2855765264201,-9.99494898233489,
-1.09527884074407E-15));
#12564=CARTESIAN_POINT('Ctrl Pts',(-13.2806858148038,-9.93745562189104,
1.18024020512711E-16));
#12565=CARTESIAN_POINT('Ctrl Pts',(-13.2786149095285,-9.87971946880946,
-1.38777878078145E-16));
#12566=CARTESIAN_POINT('Ctrl Pts',(-13.2775754853061,-9.85074066579963,
-2.67671322386771E-16));
#12567=CARTESIAN_POINT('Ctrl Pts',(-13.2772469104407,-9.82170053398399,
1.4948294717503E-15));
#12568=CARTESIAN_POINT('Ctrl Pts',(-13.2776249668018,-9.79262525364946,
1.63757896132211E-15));
#12569=CARTESIAN_POINT('Ctrl Pts',(-13.2777973926671,-9.77936445211961,
1.70268487355815E-15));
#12570=CARTESIAN_POINT('Ctrl Pts',(-13.2781170152694,-9.76609462368694,
-4.7430123169196E-16));
#12571=CARTESIAN_POINT('Ctrl Pts',(-13.2785824498934,-9.75283980605701,
-5.27355936696949E-16));
#12572=CARTESIAN_POINT('Ctrl Pts',(-13.280933076777,-9.68589779304374,-7.95302946759129E-16));
#12573=CARTESIAN_POINT('Ctrl Pts',(-13.2869992525162,-9.61921855261629,
1.59603393177068E-15));
#12574=CARTESIAN_POINT('Ctrl Pts',(-13.2966473181584,-9.55313456281087,
1.49880108324396E-15));
#12575=CARTESIAN_POINT('Ctrl Pts',(-13.3064659127467,-9.4858825426913,1.39984965030756E-15));
#12576=CARTESIAN_POINT('Ctrl Pts',(-13.3199939979885,-9.41924600106486,
3.7367831032364E-16));
#12577=CARTESIAN_POINT('Ctrl Pts',(-13.3371419608068,-9.35355952774662,
2.4980018054066E-16));
#12578=CARTESIAN_POINT('Ctrl Pts',(-13.3514852540965,-9.29861653761111,
1.46183187287034E-16));
#12579=CARTESIAN_POINT('Ctrl Pts',(-13.3683620550236,-9.24433764320676,
4.21405766872162E-17));
#12580=CARTESIAN_POINT('Ctrl Pts',(-13.3877476280939,-9.19091835353792,
-2.77555756156289E-16));
#12581=CARTESIAN_POINT('Ctrl Pts',(-13.39668378758,-9.16629368598843,-4.24926040595927E-16));
#12582=CARTESIAN_POINT('Ctrl Pts',(-13.4061533950394,-9.14185172195395,
7.07869180218989E-16));
#12583=CARTESIAN_POINT('Ctrl Pts',(-13.4161558307215,-9.11761203383739,
6.93889390390723E-16));
#12584=CARTESIAN_POINT('Ctrl Pts',(-13.4205143377574,-9.10704972136054,
6.87797772882415E-16));
#12585=CARTESIAN_POINT('Ctrl Pts',(-13.4249739997542,-9.09652612469906,
-3.22868594808326E-17));
#12586=CARTESIAN_POINT('Ctrl Pts',(-13.4295289897423,-9.08605561214841,
-5.55111512312578E-17));
#12587=CARTESIAN_POINT('Ctrl Pts',(-13.4575216444335,-9.02170916066706,
-1.98235851199708E-16));
#12588=CARTESIAN_POINT('Ctrl Pts',(-13.489160585127,-8.95924403457073,-2.25359481219569E-15));
#12589=CARTESIAN_POINT('Ctrl Pts',(-13.524338957658,-8.8990088207193,-1.98452365651747E-15));
#12590=CARTESIAN_POINT('Ctrl Pts',(-13.5557936925823,-8.84514951602471,
-1.74393373524742E-15));
#12591=CARTESIAN_POINT('Ctrl Pts',(-13.590078948554,-8.79307231810761,5.85737278460583E-16));
#12592=CARTESIAN_POINT('Ctrl Pts',(-13.627153472105,-8.74302986930091,1.12410081243297E-15));
#12593=CARTESIAN_POINT('Ctrl Pts',(-13.6675383362097,-8.68851918916382,
1.70977456371544E-15));
#12594=CARTESIAN_POINT('Ctrl Pts',(-13.7112321890346,-8.63642161961057,
1.4217873119626E-15));
#12595=CARTESIAN_POINT('Ctrl Pts',(-13.7579211246953,-8.58682326989449,
1.22124532708767E-15));
#12596=CARTESIAN_POINT('Ctrl Pts',(-13.7759302268488,-8.56769193322904,
1.14389121651416E-15));
#12597=CARTESIAN_POINT('Ctrl Pts',(-13.7943854276088,-8.54893272295167,
2.44014659021857E-15));
#12598=CARTESIAN_POINT('Ctrl Pts',(-13.8132703795349,-8.53055173814469,
2.44249065417534E-15));
#12599=CARTESIAN_POINT('Ctrl Pts',(-13.8215560161117,-8.52248721350985,
2.44351909534558E-15));
#12600=CARTESIAN_POINT('Ctrl Pts',(-13.8299240193705,-8.5144959821821,-9.50368270547519E-16));
#12601=CARTESIAN_POINT('Ctrl Pts',(-13.838363019459,-8.50658761589045,-9.57567358739198E-16));
#12602=CARTESIAN_POINT('Ctrl Pts',(-13.8893887557786,-8.45877031420949,
-1.00109606734903E-15));
#12603=CARTESIAN_POINT('Ctrl Pts',(-13.9430963123383,-8.4138917808739,-6.40189758604347E-17));
#12604=CARTESIAN_POINT('Ctrl Pts',(-13.9991087396997,-8.37201357687976,
3.19189119579733E-16));
#12605=CARTESIAN_POINT('Ctrl Pts',(-14.0564211033334,-8.32916346363337,
7.11290707528551E-16));
#12606=CARTESIAN_POINT('Ctrl Pts',(-14.1161471900346,-8.28945395175835,
1.00414780997289E-15));
#12607=CARTESIAN_POINT('Ctrl Pts',(-14.1779321771154,-8.25297867940102,
2.02615701994091E-15));
#12608=CARTESIAN_POINT('Ctrl Pts',(-14.2252015423102,-8.22507282312259,
2.80805775118726E-15));
#12609=CARTESIAN_POINT('Ctrl Pts',(-14.2736771332203,-8.19906053178973,
2.53848381353579E-15));
#12610=CARTESIAN_POINT('Ctrl Pts',(-14.3232149985245,-8.17499768689248,
2.74780198594726E-15));
#12611=CARTESIAN_POINT('Ctrl Pts',(-14.3540407103556,-8.16002420513092,
2.8780534940441E-15));
#12612=CARTESIAN_POINT('Ctrl Pts',(-14.3852779880121,-8.1458058278048,1.08257402890549E-15));
#12613=CARTESIAN_POINT('Ctrl Pts',(-14.4168940263936,-8.13235879193744,
1.13103970633688E-15));
#12614=CARTESIAN_POINT('Ctrl Pts',(-14.4346636982448,-8.12480093753923,
1.15827965251909E-15));
#12615=CARTESIAN_POINT('Ctrl Pts',(-14.4525590851067,-8.11748457270256,
1.14587934816188E-15));
#12616=CARTESIAN_POINT('Ctrl Pts',(-14.470541741264,-8.11042529656637,1.04777297948999E-15));
#12617=CARTESIAN_POINT('Ctrl Pts',(-14.5401796653021,-8.08308821515669,
6.67855586339259E-16));
#12618=CARTESIAN_POINT('Ctrl Pts',(-14.611192923579,-8.05957098628127,1.41062069047362E-15));
#12619=CARTESIAN_POINT('Ctrl Pts',(-14.683209836623,-8.03998786369269,1.49880108324396E-15));
#12620=CARTESIAN_POINT('Ctrl Pts',(-14.7370845758773,-8.02533803244261,
1.56476747179147E-15));
#12621=CARTESIAN_POINT('Ctrl Pts',(-14.7915219476125,-8.01289052704023,
-7.21547261836267E-16));
#12622=CARTESIAN_POINT('Ctrl Pts',(-14.8463769008119,-8.00270909147673,
-6.76542155630955E-16));
#12623=CARTESIAN_POINT('Ctrl Pts',(-14.8634609622712,-7.99953817871924,
-6.62525736774458E-16));
#12624=CARTESIAN_POINT('Ctrl Pts',(-14.8805855769004,-7.99658717289818,
-1.00648135721956E-15));
#12625=CARTESIAN_POINT('Ctrl Pts',(-14.8977464806917,-7.99385830531565,
-1.14491749414469E-15));
#12626=CARTESIAN_POINT('Ctrl Pts',(-14.9143450340983,-7.9912188607468,-1.27881717915669E-15));
#12627=CARTESIAN_POINT('Ctrl Pts',(-14.9309690935528,-7.98878863041095,
-2.06502921266531E-15));
#12628=CARTESIAN_POINT('Ctrl Pts',(-14.9476086519096,-7.98656978706703,
-2.17534323887492E-15));
#12629=CARTESIAN_POINT('Ctrl Pts',(-15.0222846677452,-7.9766119277817,-2.67041719405268E-15));
#12630=CARTESIAN_POINT('Ctrl Pts',(-15.0973087342006,-7.97090191711569,
-8.83830117641646E-17));
#12631=CARTESIAN_POINT('Ctrl Pts',(-15.1723238725507,-7.96957800273067,
4.04190569902596E-16));
#12632=CARTESIAN_POINT('Ctrl Pts',(-15.2297781588663,-7.96856401331724,
7.81453935871769E-16));
#12633=CARTESIAN_POINT('Ctrl Pts',(-15.28722791073,-7.97012372441746,1.62407242976159E-15));
#12634=CARTESIAN_POINT('Ctrl Pts',(-15.3445186506179,-7.9743391343232,1.55257751099924E-15));
#12635=CARTESIAN_POINT('Ctrl Pts',(-15.3577644165905,-7.97531374790297,
1.53951714939913E-15));
#12636=CARTESIAN_POINT('Ctrl Pts',(-15.3710016931801,-7.97643039983451,
9.09140411173112E-16));
#12637=CARTESIAN_POINT('Ctrl Pts',(-15.3842290239278,-7.97768774796568,
9.0205620750794E-16));
#12638=CARTESIAN_POINT('Ctrl Pts',(-16.6638186297495,-9.99906044123799,
7.37851963660979));
#12639=CARTESIAN_POINT('Ctrl Pts',(-16.6649348408491,-9.78304620021843,
7.36411833671163));
#12640=CARTESIAN_POINT('Ctrl Pts',(-16.6258964811017,-9.56741857858544,
7.34971703681347));
#12641=CARTESIAN_POINT('Ctrl Pts',(-16.5448315551234,-9.36895973630092,
7.33531573691531));
#12642=CARTESIAN_POINT('Ctrl Pts',(-16.3362936925395,-8.85842842721179,
7.29826868773897));
#12643=CARTESIAN_POINT('Ctrl Pts',(-15.849638685014,-8.46151410667921,7.26122163856263));
#12644=CARTESIAN_POINT('Ctrl Pts',(-15.3076109613776,-8.3598583906821,7.22417458938629));
#12645=CARTESIAN_POINT('Ctrl Pts',(-14.7655832377413,-8.25820267468499,
7.18712754020995));
#12646=CARTESIAN_POINT('Ctrl Pts',(-14.1681827979942,-8.45180556322336,
7.15008049103361));
#12647=CARTESIAN_POINT('Ctrl Pts',(-13.7888217959707,-8.85206824290433,
7.11303344185727));
#12648=CARTESIAN_POINT('Ctrl Pts',(-13.4094607939473,-9.25233092258531,
7.07598639268093));
#12649=CARTESIAN_POINT('Ctrl Pts',(-13.2481392296476,-9.8592533934089,7.03893934350459));
#12650=CARTESIAN_POINT('Ctrl Pts',(-13.3786940021983,-10.3950543874535,
7.00189229432825));
#12651=CARTESIAN_POINT('Ctrl Pts',(-13.509248774749,-10.9308553814982,6.96484524515191));
#12652=CARTESIAN_POINT('Ctrl Pts',(-13.9316798841501,-11.3955348987639,
6.92779819597557));
#12653=CARTESIAN_POINT('Ctrl Pts',(-14.4526473070119,-11.5764208125474,
6.89075114679923));
#12654=CARTESIAN_POINT('Ctrl Pts',(-14.9736147298738,-11.7573067263309,
6.85370409762289));
#12655=CARTESIAN_POINT('Ctrl Pts',(-15.5931184661963,-11.6543990366322,
6.81665704844655));
#12656=CARTESIAN_POINT('Ctrl Pts',(-16.0276247561321,-11.3147952675694,
6.77960999927021));
#12657=CARTESIAN_POINT('Ctrl Pts',(-16.422837505005,-11.0059027562118,6.74591321171674));
#12658=CARTESIAN_POINT('Ctrl Pts',(-16.6649994941594,-10.5011885431139,
6.71221642416327));
#12659=CARTESIAN_POINT('Ctrl Pts',(-16.6681788248613,-9.99913246376521,
6.6785196366098));
#12660=CARTESIAN_POINT('Ctrl Pts',(-15.5301702171886,-11.9851743256717,
8.));
#12661=CARTESIAN_POINT('Ctrl Pts',(-15.6001784614245,-11.9592528683504,
8.));
#12662=CARTESIAN_POINT('Ctrl Pts',(-15.6685003286655,-11.9292588432449,
8.));
#12663=CARTESIAN_POINT('Ctrl Pts',(-15.7349164951987,-11.895479109407,8.));
#12664=CARTESIAN_POINT('Ctrl Pts',(-15.7995895967044,-11.8625859108175,
8.));
#12665=CARTESIAN_POINT('Ctrl Pts',(-15.8624561372199,-11.8261021803305,
8.));
#12666=CARTESIAN_POINT('Ctrl Pts',(-15.9232826782083,-11.7862589889858,
8.));
#12667=CARTESIAN_POINT('Ctrl Pts',(-15.9368593447254,-11.7773658690899,
8.));
#12668=CARTESIAN_POINT('Ctrl Pts',(-15.9503360255514,-11.7683040401431,
8.));
#12669=CARTESIAN_POINT('Ctrl Pts',(-15.9637041645642,-11.7590798556399,
8.));
#12670=CARTESIAN_POINT('Ctrl Pts',(-16.0250458750272,-11.7167533018461,
8.));
#12671=CARTESIAN_POINT('Ctrl Pts',(-16.0839844344716,-11.6710958663792,
8.));
#12672=CARTESIAN_POINT('Ctrl Pts',(-16.1402812498345,-11.6223768930558,
8.));
#12673=CARTESIAN_POINT('Ctrl Pts',(-16.179806333597,-11.5881720896576,8.));
#12674=CARTESIAN_POINT('Ctrl Pts',(-16.2180285241833,-11.5524573236335,
8.));
#12675=CARTESIAN_POINT('Ctrl Pts',(-16.2548523907682,-11.5153174086833,
8.));
#12676=CARTESIAN_POINT('Ctrl Pts',(-16.2688610567185,-11.5011885104928,
8.));
#12677=CARTESIAN_POINT('Ctrl Pts',(-16.2826672344801,-11.4868533051394,
8.));
#12678=CARTESIAN_POINT('Ctrl Pts',(-16.2962652100924,-11.4723162794782,
8.));
#12679=CARTESIAN_POINT('Ctrl Pts',(-16.3091901141748,-11.4584988063725,
8.));
#12680=CARTESIAN_POINT('Ctrl Pts',(-16.3219307389119,-11.4444944578142,
8.));
#12681=CARTESIAN_POINT('Ctrl Pts',(-16.3344601775897,-11.430332285647,8.));
#12682=CARTESIAN_POINT('Ctrl Pts',(-16.3825592602788,-11.3759653257495,
8.));
#12683=CARTESIAN_POINT('Ctrl Pts',(-16.4276039061328,-11.3192201229115,
8.));
#12684=CARTESIAN_POINT('Ctrl Pts',(-16.4693715627496,-11.2603446276274,
8.));
#12685=CARTESIAN_POINT('Ctrl Pts',(-16.5102413201592,-11.2027348069065,
8.));
#12686=CARTESIAN_POINT('Ctrl Pts',(-16.5479738235429,-11.1430844349936,
8.));
#12687=CARTESIAN_POINT('Ctrl Pts',(-16.5823154377681,-11.0816066782684,
8.));
#12688=CARTESIAN_POINT('Ctrl Pts',(-16.6159042787281,-11.0214765230673,
8.));
#12689=CARTESIAN_POINT('Ctrl Pts',(-16.6462495368313,-10.9595975009557,
8.));
#12690=CARTESIAN_POINT('Ctrl Pts',(-16.6730656532177,-10.8961620666141,
8.));
#12691=CARTESIAN_POINT('Ctrl Pts',(-16.6817772278961,-10.8755542158888,
8.));
#12692=CARTESIAN_POINT('Ctrl Pts',(-16.6901159465972,-10.854782095613,8.));
#12693=CARTESIAN_POINT('Ctrl Pts',(-16.6980708146011,-10.8338523288304,
8.));
#12694=CARTESIAN_POINT('Ctrl Pts',(-16.7025652307942,-10.8220272322104,
8.));
#12695=CARTESIAN_POINT('Ctrl Pts',(-16.7069374588343,-10.810150529649,8.));
#12696=CARTESIAN_POINT('Ctrl Pts',(-16.7111796927613,-10.7982404031086,
8.));
#12697=CARTESIAN_POINT('Ctrl Pts',(-16.7340960329223,-10.7339024821311,
8.));
#12698=CARTESIAN_POINT('Ctrl Pts',(-16.7532665659449,-10.6684789076532,
8.));
#12699=CARTESIAN_POINT('Ctrl Pts',(-16.7684629972282,-10.6021691817607,
8.));
#12700=CARTESIAN_POINT('Ctrl Pts',(-16.7706603748747,-10.5925809102312,
8.));
#12701=CARTESIAN_POINT('Ctrl Pts',(-16.772774571369,-10.582974096752,8.));
#12702=CARTESIAN_POINT('Ctrl Pts',(-16.7748048055191,-10.5733493334729,
8.));
#12703=CARTESIAN_POINT('Ctrl Pts',(-16.7891234309595,-10.5054687984451,
8.));
#12704=CARTESIAN_POINT('Ctrl Pts',(-16.799269982444,-10.4366949085313,8.));
#12705=CARTESIAN_POINT('Ctrl Pts',(-16.805341122567,-10.367383506366,8.));
#12706=CARTESIAN_POINT('Ctrl Pts',(-16.8110051473463,-10.3027199520097,
8.));
#12707=CARTESIAN_POINT('Ctrl Pts',(-16.8131212227444,-10.2375878497544,
8.));
#12708=CARTESIAN_POINT('Ctrl Pts',(-16.8117296898732,-10.1722884874833,
8.));
#12709=CARTESIAN_POINT('Ctrl Pts',(-16.8114208851943,-10.1577974545929,
8.));
#12710=CARTESIAN_POINT('Ctrl Pts',(-16.8109392074865,-10.1432982578336,
8.));
#12711=CARTESIAN_POINT('Ctrl Pts',(-16.8102848748653,-10.1287943297925,
8.));
#12712=CARTESIAN_POINT('Ctrl Pts',(-16.8097776518725,-10.117551231788,8.));
#12713=CARTESIAN_POINT('Ctrl Pts',(-16.8091666413548,-10.1063061788777,
8.));
#12714=CARTESIAN_POINT('Ctrl Pts',(-16.8084530036145,-10.0950735021604,
8.));
#12715=CARTESIAN_POINT('Ctrl Pts',(-16.8041172567116,-10.0268287323881,
8.));
#12716=CARTESIAN_POINT('Ctrl Pts',(-16.7959924597437,-9.95891461918857,
8.));
#12717=CARTESIAN_POINT('Ctrl Pts',(-16.7841888730333,-9.89166697312925,
8.));
#12718=CARTESIAN_POINT('Ctrl Pts',(-16.7724402253421,-9.82473232682209,
8.));
#12719=CARTESIAN_POINT('Ctrl Pts',(-16.757046467,-9.75845693091033,8.));
#12720=CARTESIAN_POINT('Ctrl Pts',(-16.7380691925747,-9.69319173096208,
8.));
#12721=CARTESIAN_POINT('Ctrl Pts',(-16.7194993974145,-9.6293279027342,8.));
#12722=CARTESIAN_POINT('Ctrl Pts',(-16.6974977885672,-9.56643054222536,
8.));
#12723=CARTESIAN_POINT('Ctrl Pts',(-16.6720845431421,-9.50486087342584,
8.));
#12724=CARTESIAN_POINT('Ctrl Pts',(-16.6666981633995,-9.4918110794608,8.));
#12725=CARTESIAN_POINT('Ctrl Pts',(-16.6611584002427,-9.47882107274358,
8.));
#12726=CARTESIAN_POINT('Ctrl Pts',(-16.6554652571167,-9.46589453727988,
8.));
#12727=CARTESIAN_POINT('Ctrl Pts',(-16.6501414525651,-9.45380660152724,
8.));
#12728=CARTESIAN_POINT('Ctrl Pts',(-16.6446827491174,-9.44177279704584,
8.));
#12729=CARTESIAN_POINT('Ctrl Pts',(-16.6390983123084,-9.42981508426328,
8.));
#12730=CARTESIAN_POINT('Ctrl Pts',(-16.6114456124069,-9.37060355507962,
8.));
#12731=CARTESIAN_POINT('Ctrl Pts',(-16.5806669470622,-9.31314722135339,
8.));
#12732=CARTESIAN_POINT('Ctrl Pts',(-16.5468263465045,-9.25775959274632,
8.));
#12733=CARTESIAN_POINT('Ctrl Pts',(-16.513630640101,-9.20342747607804,8.));
#12734=CARTESIAN_POINT('Ctrl Pts',(-16.4774880716359,-9.15108525442289,
8.));
#12735=CARTESIAN_POINT('Ctrl Pts',(-16.4384245194448,-9.10106457909364,
8.));
#12736=CARTESIAN_POINT('Ctrl Pts',(-16.4006314655837,-9.05267077026559,
8.));
#12737=CARTESIAN_POINT('Ctrl Pts',(-16.3601038589244,-9.0064494922551,8.));
#12738=CARTESIAN_POINT('Ctrl Pts',(-16.3168397930964,-8.96274315872729,
8.));
#12739=CARTESIAN_POINT('Ctrl Pts',(-16.309631880704,-8.95546156331935,8.));
#12740=CARTESIAN_POINT('Ctrl Pts',(-16.3023479643107,-8.94824988022331,
8.));
#12741=CARTESIAN_POINT('Ctrl Pts',(-16.2949879778178,-8.9411098246742,8.));
#12742=CARTESIAN_POINT('Ctrl Pts',(-16.2872273416651,-8.93358109166894,
8.));
#12743=CARTESIAN_POINT('Ctrl Pts',(-16.2793821269318,-8.92613199722373,
8.));
#12744=CARTESIAN_POINT('Ctrl Pts',(-16.2714538290145,-8.91876328587892,
8.));
#12745=CARTESIAN_POINT('Origin',(0.,0.,0.));
#12746=CARTESIAN_POINT('',(-20.,10.,0.));
#12747=CARTESIAN_POINT('',(-20.,-14.,0.));
#12748=CARTESIAN_POINT('',(-20.,10.,0.));
#12749=CARTESIAN_POINT('',(-16.,14.,0.));
#12750=CARTESIAN_POINT('',(-16.,14.,0.));
#12751=CARTESIAN_POINT('',(16.,14.,0.));
#12752=CARTESIAN_POINT('',(16.,14.,0.));
#12753=CARTESIAN_POINT('',(20.,10.,0.));
#12754=CARTESIAN_POINT('',(20.,10.,0.));
#12755=CARTESIAN_POINT('',(20.,-14.,0.));
#12756=CARTESIAN_POINT('',(20.,-14.,0.));
#12757=CARTESIAN_POINT('',(-20.,-14.,0.));
#12758=CARTESIAN_POINT('',(-10.,-6.,0.));
#12759=CARTESIAN_POINT('',(-6.,-6.,0.));
#12760=CARTESIAN_POINT('',(-3.,-6.,0.));
#12761=CARTESIAN_POINT('',(-6.,-4.,0.));
#12762=CARTESIAN_POINT('',(-6.,-2.,0.));
#12763=CARTESIAN_POINT('',(-10.,-4.,0.));
#12764=CARTESIAN_POINT('',(-5.,-4.,0.));
#12765=CARTESIAN_POINT('',(-10.,-3.,0.));
#12766=CARTESIAN_POINT('',(6.,-6.,0.));
#12767=CARTESIAN_POINT('',(10.,-6.,0.));
#12768=CARTESIAN_POINT('',(5.,-6.,0.));
#12769=CARTESIAN_POINT('',(10.,-4.,0.));
#12770=CARTESIAN_POINT('',(10.,-2.,0.));
#12771=CARTESIAN_POINT('',(6.,-4.,0.));
#12772=CARTESIAN_POINT('',(3.,-4.,0.));
#12773=CARTESIAN_POINT('',(6.,-3.,0.));
#12774=CARTESIAN_POINT('',(-2.,4.,0.));
#12775=CARTESIAN_POINT('',(2.,4.,0.));
#12776=CARTESIAN_POINT('',(1.,4.,0.));
#12777=CARTESIAN_POINT('',(2.,6.,0.));
#12778=CARTESIAN_POINT('',(2.,3.,0.));
#12779=CARTESIAN_POINT('',(-2.,6.,0.));
#12780=CARTESIAN_POINT('',(-1.,6.,0.));
#12781=CARTESIAN_POINT('',(-2.,2.,0.));
#12782=CARTESIAN_POINT('Ctrl Pts',(13.6609982804014,-8.44145197141313,-1.11022302462516E-15));
#12783=CARTESIAN_POINT('Ctrl Pts',(13.6101587658985,-8.49415672193897,-1.06794690886987E-15));
#12784=CARTESIAN_POINT('Ctrl Pts',(13.5625411139953,-8.54962577124122,2.88974792760603E-16));
#12785=CARTESIAN_POINT('Ctrl Pts',(13.5181882608598,-8.60751250695679,-1.11022302462516E-16));
#12786=CARTESIAN_POINT('Ctrl Pts',(13.4726056590943,-8.66700423826799,-5.22109910359462E-16));
#12787=CARTESIAN_POINT('Ctrl Pts',(13.4304710124629,-8.72905053741109,-2.35827857905889E-15));
#12788=CARTESIAN_POINT('Ctrl Pts',(13.3918784169615,-8.79330181954066,-3.3584246494911E-15));
#12789=CARTESIAN_POINT('Ctrl Pts',(13.3592682533102,-8.84759318807451,-4.20353305974852E-15));
#12790=CARTESIAN_POINT('Ctrl Pts',(13.3291878694,-8.90345971497981,-1.99390072014143E-15));
#12791=CARTESIAN_POINT('Ctrl Pts',(13.3017223445621,-8.96069685037408,-2.05391259555654E-15));
#12792=CARTESIAN_POINT('Ctrl Pts',(13.2895237825855,-8.9861182012344,-2.08056632185161E-15));
#12793=CARTESIAN_POINT('Ctrl Pts',(13.2778413813041,-9.01180994946495,-6.14394228437601E-16));
#12794=CARTESIAN_POINT('Ctrl Pts',(13.2666843062596,-9.03775415254288,-6.66133814775094E-16));
#12795=CARTESIAN_POINT('Ctrl Pts',(13.2605517074626,-9.0520146453648,-6.94573000105211E-16));
#12796=CARTESIAN_POINT('Ctrl Pts',(13.2545778422614,-9.06635140970031,5.42362793670161E-16));
#12797=CARTESIAN_POINT('Ctrl Pts',(13.2487643717516,-9.08076144522329,5.82867087928207E-16));
#12798=CARTESIAN_POINT('Ctrl Pts',(13.2434046675288,-9.09404671571921,6.20209848437461E-16));
#12799=CARTESIAN_POINT('Ctrl Pts',(13.238180662491,-9.10739625085751,-2.23585955336618E-15));
#12800=CARTESIAN_POINT('Ctrl Pts',(13.2331012669984,-9.12078688698765,-2.13717932240343E-15));
#12801=CARTESIAN_POINT('Ctrl Pts',(13.2071398037565,-9.18922820213755,-1.63281158955259E-15));
#12802=CARTESIAN_POINT('Ctrl Pts',(13.1849033194385,-9.25885913230428,-1.93388574546088E-15));
#12803=CARTESIAN_POINT('Ctrl Pts',(13.166476514568,-9.32935142061032,-1.60982338570648E-15));
#12804=CARTESIAN_POINT('Ctrl Pts',(13.1481932910496,-9.39929443419718,-1.28828611438278E-15));
#12805=CARTESIAN_POINT('Ctrl Pts',(13.1336605333199,-9.47008645034364,-1.68393081631434E-15));
#12806=CARTESIAN_POINT('Ctrl Pts',(13.1230118477655,-9.54140923520067,-2.1094237467878E-15));
#12807=CARTESIAN_POINT('Ctrl Pts',(13.1141608028635,-9.6006917793311,-2.46308777545049E-15));
#12808=CARTESIAN_POINT('Ctrl Pts',(13.107994013581,-9.66034132438599,-1.11721423492157E-15));
#12809=CARTESIAN_POINT('Ctrl Pts',(13.1046159053985,-9.72016898875187,-1.13797860024079E-15));
#12810=CARTESIAN_POINT('Ctrl Pts',(13.1032060629936,-9.74513786886308,-1.14664454021581E-15));
#12811=CARTESIAN_POINT('Ctrl Pts',(13.1022822552789,-9.7701376692114,2.01322589821468E-15));
#12812=CARTESIAN_POINT('Ctrl Pts',(13.1018534077158,-9.7951541096622,2.38697950294409E-15));
#12813=CARTESIAN_POINT('Ctrl Pts',(13.1016548070149,-9.80673930457659,2.56006601256404E-15));
#12814=CARTESIAN_POINT('Ctrl Pts',(13.1015623689196,-9.8183280627853,4.77538944853251E-16));
#12815=CARTESIAN_POINT('Ctrl Pts',(13.1015770379907,-9.82991893585887,6.10622663543836E-16));
#12816=CARTESIAN_POINT('Ctrl Pts',(13.1015923232661,-9.84199670727381,7.49296836161562E-16));
#12817=CARTESIAN_POINT('Ctrl Pts',(13.1017239212966,-9.85406846363438,-1.57579408396219E-15));
#12818=CARTESIAN_POINT('Ctrl Pts',(13.1019722848962,-9.86612818157873,-1.52655665885959E-15));
#12819=CARTESIAN_POINT('Ctrl Pts',(13.1033874555188,-9.93484420350411,-1.24600283508758E-15));
#12820=CARTESIAN_POINT('Ctrl Pts',(13.1085897217447,-10.0032172387899,-5.54350890407896E-16));
#12821=CARTESIAN_POINT('Ctrl Pts',(13.1176919287551,-10.0709665059013,-3.05311331771918E-16));
#12822=CARTESIAN_POINT('Ctrl Pts',(13.1259447254805,-10.1323934685191,-7.95119348054797E-17));
#12823=CARTESIAN_POINT('Ctrl Pts',(13.1374040930353,-10.1933080511867,1.4078718797507E-15));
#12824=CARTESIAN_POINT('Ctrl Pts',(13.1521893955025,-10.2534893792597,1.73472347597681E-15));
#12825=CARTESIAN_POINT('Ctrl Pts',(13.1696761947384,-10.3246667396211,2.121295766655E-15));
#12826=CARTESIAN_POINT('Ctrl Pts',(13.1918154833854,-10.3948200423067,3.90173504212154E-16));
#12827=CARTESIAN_POINT('Ctrl Pts',(13.2183556262969,-10.463600226698,1.38777878078145E-16));
#12828=CARTESIAN_POINT('Ctrl Pts',(13.2242000202031,-10.478746282688,8.34181511049387E-17));
#12829=CARTESIAN_POINT('Ctrl Pts',(13.2302579878528,-10.4938255820364,1.17983157929043E-15));
#12830=CARTESIAN_POINT('Ctrl Pts',(13.2365271040103,-10.5088340883018,1.27675647831893E-15));
#12831=CARTESIAN_POINT('Ctrl Pts',(13.2429827911969,-10.5242892528182,1.37656589530753E-15));
#12832=CARTESIAN_POINT('Ctrl Pts',(13.249665027142,-10.5396748622705,1.08718752268941E-15));
#12833=CARTESIAN_POINT('Ctrl Pts',(13.2565569191837,-10.5549556510553,1.04083408558608E-15));
#12834=CARTESIAN_POINT('Ctrl Pts',(13.284756021213,-10.6174790509322,8.51172771336908E-16));
#12835=CARTESIAN_POINT('Ctrl Pts',(13.3164923441765,-10.6783312930776,2.50909797921603E-15));
#12836=CARTESIAN_POINT('Ctrl Pts',(13.3515101424189,-10.7372595582005,2.26207941267376E-15));
#12837=CARTESIAN_POINT('Ctrl Pts',(13.386520648505,-10.7961755520174,2.01511228563007E-15));
#12838=CARTESIAN_POINT('Ctrl Pts',(13.4248121377808,-10.8531691394787,-1.01449280433253E-15));
#12839=CARTESIAN_POINT('Ctrl Pts',(13.4661672023612,-10.9079526014265,-9.99200722162641E-16));
#12840=CARTESIAN_POINT('Ctrl Pts',(13.4961034954915,-10.9476095042072,-9.88131019840704E-16));
#12841=CARTESIAN_POINT('Ctrl Pts',(13.5276459606208,-10.9861075874816,1.68431897089301E-15));
#12842=CARTESIAN_POINT('Ctrl Pts',(13.5607207523854,-11.0233228320109,2.00534033822919E-15));
#12843=CARTESIAN_POINT('Ctrl Pts',(13.5855273390455,-11.0512348199399,2.246111147165E-15));
#12844=CARTESIAN_POINT('Ctrl Pts',(13.6111960512469,-11.07842493416,-3.45593041235091E-16));
#12845=CARTESIAN_POINT('Ctrl Pts',(13.6376974486013,-11.1048353845436,-5.48172618408671E-16));
#12846=CARTESIAN_POINT('Ctrl Pts',(13.646504369492,-11.1136120820175,-6.15493684025071E-16));
#12847=CARTESIAN_POINT('Ctrl Pts',(13.6553963636123,-11.1222957620102,-1.38096788297345E-15));
#12848=CARTESIAN_POINT('Ctrl Pts',(13.6643717837757,-11.1308844426468,-1.19348975147204E-15));
#12849=CARTESIAN_POINT('Ctrl Pts',(13.7119764880025,-11.1764379202511,-1.99125049143139E-16));
#12850=CARTESIAN_POINT('Ctrl Pts',(13.7619290644544,-11.2193251985614,1.6044485410188E-16));
#12851=CARTESIAN_POINT('Ctrl Pts',(13.8140392685458,-11.2592667110007,-3.2612801348364E-16));
#12852=CARTESIAN_POINT('Ctrl Pts',(13.8507160970753,-11.287378825096,-6.68593562078286E-16));
#12853=CARTESIAN_POINT('Ctrl Pts',(13.8884623109934,-11.3140308200616,9.18435597775855E-16));
#12854=CARTESIAN_POINT('Ctrl Pts',(13.927216032338,-11.3391104485778,-4.5102810375397E-17));
#12855=CARTESIAN_POINT('Ctrl Pts',(13.9396521575986,-11.3471585376618,-3.54303679903529E-16));
#12856=CARTESIAN_POINT('Ctrl Pts',(13.9521937968018,-11.3550456673736,-3.44690438430398E-16));
#12857=CARTESIAN_POINT('Ctrl Pts',(13.9648333834986,-11.3627644446501,-1.42247325030098E-16));
#12858=CARTESIAN_POINT('Ctrl Pts',(14.018677675764,-11.3956462239028,7.20154779289231E-16));
#12859=CARTESIAN_POINT('Ctrl Pts',(14.0741898030955,-11.4254114396644,4.93984524176593E-16));
#12860=CARTESIAN_POINT('Ctrl Pts',(14.1312019479731,-11.4517907289967,1.56125112837913E-15));
#12861=CARTESIAN_POINT('Ctrl Pts',(14.1837968166844,-11.4761261624751,2.54582638069662E-15));
#12862=CARTESIAN_POINT('Ctrl Pts',(14.23766883648,-11.4975798614081,-2.36021162522633E-16));
#12863=CARTESIAN_POINT('Ctrl Pts',(14.2926912967956,-11.5159012511454,3.64725610824124E-16));
#12864=CARTESIAN_POINT('Ctrl Pts',(14.3029516288356,-11.5193177385409,4.87279518509108E-16));
#12865=CARTESIAN_POINT('Ctrl Pts',(14.3132519680667,-11.5226251912698,1.24120044379145E-15));
#12866=CARTESIAN_POINT('Ctrl Pts',(14.3235906297078,-11.5258236994894,1.26287869051112E-15));
#12867=CARTESIAN_POINT('Ctrl Pts',(16.6117095221421,-10.4218393251423,0.));
#12868=CARTESIAN_POINT('Ctrl Pts',(16.6342056422671,-10.3640626285304,1.03253723969441E-17));
#12869=CARTESIAN_POINT('Ctrl Pts',(16.6531280196217,-10.3051560572626,9.85900667902734E-16));
#12870=CARTESIAN_POINT('Ctrl Pts',(16.668627359564,-10.2454298235342,9.71445146547012E-16));
#12871=CARTESIAN_POINT('Ctrl Pts',(16.6851480739499,-10.1817677545397,9.56037036233499E-16));
#12872=CARTESIAN_POINT('Ctrl Pts',(16.6977802955953,-10.1171739101123,-1.65277777837953E-15));
#12873=CARTESIAN_POINT('Ctrl Pts',(16.7066568337424,-10.0519871771322,-2.33146835171283E-15));
#12874=CARTESIAN_POINT('Ctrl Pts',(16.7144238046212,-9.99494878577466,-2.92532260337946E-15));
#12875=CARTESIAN_POINT('Ctrl Pts',(16.7193145800233,-9.93745546561697,6.8060116455104E-16));
#12876=CARTESIAN_POINT('Ctrl Pts',(16.7213855572738,-9.8797193559252,6.10622663543836E-16));
#12877=CARTESIAN_POINT('Ctrl Pts',(16.7224250203391,-9.85074049893983,5.75499116364019E-16));
#12878=CARTESIAN_POINT('Ctrl Pts',(16.7227536323972,-9.8217003136112,-1.02322656074148E-15));
#12879=CARTESIAN_POINT('Ctrl Pts',(16.7223756111595,-9.79262498025395,-1.52655665885959E-15));
#12880=CARTESIAN_POINT('Ctrl Pts',(16.722203203288,-9.77936430641241,-1.75611537737089E-15));
#12881=CARTESIAN_POINT('Ctrl Pts',(16.7218836016271,-9.76609460618316,6.45474011158562E-16));
#12882=CARTESIAN_POINT('Ctrl Pts',(16.7214181907915,-9.75283991662234,5.82867087928207E-16));
#12883=CARTESIAN_POINT('Ctrl Pts',(16.7190676596557,-9.68589785571542,2.66674358641745E-16));
#12884=CARTESIAN_POINT('Ctrl Pts',(16.7130015751494,-9.61921857039721,-3.30153071919369E-15));
#12885=CARTESIAN_POINT('Ctrl Pts',(16.7033535912675,-9.55313453802705,-2.60902410786912E-15));
#12886=CARTESIAN_POINT('Ctrl Pts',(16.6935350874628,-9.4858825264979,-1.90427803020938E-15));
#12887=CARTESIAN_POINT('Ctrl Pts',(16.6800070889265,-9.41924599491758,2.56425075671755E-15));
#12888=CARTESIAN_POINT('Ctrl Pts',(16.6628592032612,-9.35355953164192,2.74780198594726E-15));
#12889=CARTESIAN_POINT('Ctrl Pts',(16.6485159926896,-9.2986166195617,2.90133193027481E-15));
#12890=CARTESIAN_POINT('Ctrl Pts',(16.6316392742217,-9.24433780152903,5.69878197833297E-16));
#12891=CARTESIAN_POINT('Ctrl Pts',(16.6122537800222,-9.19091858497507,8.04911692853238E-16));
#12892=CARTESIAN_POINT('Ctrl Pts',(16.6033176258644,-9.16629386562554,9.13255360655956E-16));
#12893=CARTESIAN_POINT('Ctrl Pts',(16.5938480192675,-9.14185185036756,1.2939697659665E-15));
#12894=CARTESIAN_POINT('Ctrl Pts',(16.583845579661,-9.11761211165287,1.19348975147204E-15));
#12895=CARTESIAN_POINT('Ctrl Pts',(16.5794871167385,-9.10704988817558,1.14970659107644E-15));
#12896=CARTESIAN_POINT('Ctrl Pts',(16.5750275002003,-9.09652638012247,1.4297108069045E-15));
#12897=CARTESIAN_POINT('Ctrl Pts',(16.5704725567595,-9.08605595522034,1.4432899320127E-15));
#12898=CARTESIAN_POINT('Ctrl Pts',(16.5424799759779,-9.02170955472239,1.52674096965357E-15));
#12899=CARTESIAN_POINT('Ctrl Pts',(16.5108410959836,-8.95924447434619,8.11841053369489E-16));
#12900=CARTESIAN_POINT('Ctrl Pts',(16.4756627651242,-8.89900929869964,6.10622663543836E-16));
#12901=CARTESIAN_POINT('Ctrl Pts',(16.4442081085769,-8.84515009856861,4.30703514785051E-16));
#12902=CARTESIAN_POINT('Ctrl Pts',(16.409922923172,-8.79307299455403,-1.06964934127292E-15));
#12903=CARTESIAN_POINT('Ctrl Pts',(16.3728484580761,-8.7430306263865,-1.69309011255336E-15));
#12904=CARTESIAN_POINT('Ctrl Pts',(16.3324636346748,-8.68852000308266,-2.37371681853972E-15));
#12905=CARTESIAN_POINT('Ctrl Pts',(16.2887698044348,-8.63642247738161,1.13943955051508E-15));
#12906=CARTESIAN_POINT('Ctrl Pts',(16.2420808769759,-8.58682415987058,1.08246744900953E-15));
#12907=CARTESIAN_POINT('Ctrl Pts',(16.2240717422292,-8.56769279764222,1.06049182633702E-15));
#12908=CARTESIAN_POINT('Ctrl Pts',(16.2056165049632,-8.54893356154431,1.05886801823215E-15));
#12909=CARTESIAN_POINT('Ctrl Pts',(16.1867315129249,-8.53055255076451,9.85322934354826E-16));
#12910=CARTESIAN_POINT('Ctrl Pts',(16.1784458604514,-8.52248801639111,9.53055565382105E-16));
#12911=CARTESIAN_POINT('Ctrl Pts',(16.1700778405889,-8.51449677522097,2.6086384421045E-15));
#12912=CARTESIAN_POINT('Ctrl Pts',(16.1616388232942,-8.50658839906083,2.60902410786912E-15));
#12913=CARTESIAN_POINT('Ctrl Pts',(16.110613081093,-8.45877112969359,2.61135600045729E-15));
#12914=CARTESIAN_POINT('Ctrl Pts',(16.0569055066012,-8.41389261610438,-1.10985713633557E-15));
#12915=CARTESIAN_POINT('Ctrl Pts',(16.0008930531355,-8.37201442081571,-6.80011602582908E-16));
#12916=CARTESIAN_POINT('Ctrl Pts',(15.9435806322954,-8.32916429367614,-2.40189980740859E-16));
#12917=CARTESIAN_POINT('Ctrl Pts',(15.8838544772616,-8.28945475968816,2.49235514291959E-15));
#12918=CARTESIAN_POINT('Ctrl Pts',(15.8220694152881,-8.25297945854376,1.84574577843932E-15));
#12919=CARTESIAN_POINT('Ctrl Pts',(15.7747998187522,-8.22507347749358,1.35104750026396E-15));
#12920=CARTESIAN_POINT('Ctrl Pts',(15.7263239837791,-8.19906107141398,1.04416537528888E-15));
#12921=CARTESIAN_POINT('Ctrl Pts',(15.6767858652511,-8.17499812306594,1.18655085756814E-15));
#12922=CARTESIAN_POINT('Ctrl Pts',(15.6459600566815,-8.1600246064804,1.2751522770456E-15));
#12923=CARTESIAN_POINT('Ctrl Pts',(15.6147226803593,-8.1458061957273,7.80813838002484E-16));
#12924=CARTESIAN_POINT('Ctrl Pts',(15.5831065420217,-8.13235912807096,4.71844785465692E-16));
#12925=CARTESIAN_POINT('Ctrl Pts',(15.5653369179383,-8.12480130001724,2.9819094265975E-16));
#12926=CARTESIAN_POINT('Ctrl Pts',(15.5474415799036,-8.11748495921732,1.28072228025138E-15));
#12927=CARTESIAN_POINT('Ctrl Pts',(15.5294589734096,-8.11042570470516,1.31838984174237E-15));
#12928=CARTESIAN_POINT('Ctrl Pts',(15.4598209192961,-8.08308858047443,1.46425833340463E-15));
#12929=CARTESIAN_POINT('Ctrl Pts',(15.3888075307889,-8.05957130809681,1.44681167701246E-15));
#12930=CARTESIAN_POINT('Ctrl Pts',(15.3167904926731,-8.03998814314756,1.67921232474555E-15));
#12931=CARTESIAN_POINT('Ctrl Pts',(15.2629156508911,-8.02533827777076,1.85306768528583E-15));
#12932=CARTESIAN_POINT('Ctrl Pts',(15.2084781793224,-8.01289073961062,7.0540273618505E-16));
#12933=CARTESIAN_POINT('Ctrl Pts',(15.1536231312556,-8.00270927344064,9.29811783123569E-16));
#12934=CARTESIAN_POINT('Ctrl Pts',(15.1365390635248,-7.99953835547088,9.99701783996981E-16));
#12935=CARTESIAN_POINT('Ctrl Pts',(15.1194144432163,-7.99658734404714,-1.52249784740926E-15));
#12936=CARTESIAN_POINT('Ctrl Pts',(15.1022535343896,-7.99385847048614,-1.51961776495568E-15));
#12937=CARTESIAN_POINT('Ctrl Pts',(15.0856549353801,-7.99121901365762,-1.51683205388155E-15));
#12938=CARTESIAN_POINT('Ctrl Pts',(15.0690308306928,-7.98878877172398,2.00705548056742E-15));
#12939=CARTESIAN_POINT('Ctrl Pts',(15.0523912277109,-7.98656991749699,1.82839854367955E-15));
#12940=CARTESIAN_POINT('Ctrl Pts',(14.977715101503,-7.9766120213578,1.02661210794354E-15));
#12941=CARTESIAN_POINT('Ctrl Pts',(14.9026909367617,-7.97090197782506,7.13283686621106E-16));
#12942=CARTESIAN_POINT('Ctrl Pts',(14.8276757175273,-7.96957803638134,3.23699400617272E-15));
#12943=CARTESIAN_POINT('Ctrl Pts',(14.7702213490998,-7.96856402588774,5.16991087269235E-15));
#12944=CARTESIAN_POINT('Ctrl Pts',(14.7127715253326,-7.97012372111896,2.66678155952208E-16));
#12945=CARTESIAN_POINT('Ctrl Pts',(14.655480726337,-7.97433912128626,1.48145384848419E-15));
#12946=CARTESIAN_POINT('Ctrl Pts',(14.6422349512898,-7.97531373227666,1.75566928754182E-15));
#12947=CARTESIAN_POINT('Ctrl Pts',(14.6289976663039,-7.97643038184829,8.63526738818194E-16));
#12948=CARTESIAN_POINT('Ctrl Pts',(14.615770327818,-7.97768772784116,8.74300631892311E-16));
#12949=CARTESIAN_POINT('Ctrl Pts',(-16.3390017195986,11.5585480285869,0.));
#12950=CARTESIAN_POINT('Ctrl Pts',(-16.3898412778797,11.5058432326767,-1.21950438921618E-16));
#12951=CARTESIAN_POINT('Ctrl Pts',(-16.4374589773482,11.4503741465571,2.81930744747739E-15));
#12952=CARTESIAN_POINT('Ctrl Pts',(-16.481811879575,11.3924873804857,1.94289029309402E-15));
#12953=CARTESIAN_POINT('Ctrl Pts',(-16.5273944957859,11.3329956649711,1.04217388485006E-15));
#12954=CARTESIAN_POINT('Ctrl Pts',(-16.5695291639216,11.2709493924853,-9.44439383800379E-17));
#12955=CARTESIAN_POINT('Ctrl Pts',(-16.6081217856935,11.2066981448109,2.4980018054066E-16));
#12956=CARTESIAN_POINT('Ctrl Pts',(-16.6407319648364,11.1524068165565,5.40681231670983E-16));
#12957=CARTESIAN_POINT('Ctrl Pts',(-16.6708123686837,11.0965403361506,-4.80669364326135E-16));
#12958=CARTESIAN_POINT('Ctrl Pts',(-16.6982779165735,11.0393032515191,-2.4980018054066E-16));
#12959=CARTESIAN_POINT('Ctrl Pts',(-16.7104764723248,11.0138819575139,-1.47261879794735E-16));
#12960=CARTESIAN_POINT('Ctrl Pts',(-16.7221588693883,10.9881902677093,-1.31648042932263E-15));
#12961=CARTESIAN_POINT('Ctrl Pts',(-16.733315942143,10.9622461243824,-1.63757896132211E-15));
#12962=CARTESIAN_POINT('Ctrl Pts',(-16.7394485566319,10.9479856249873,-1.81407449496283E-15));
#12963=CARTESIAN_POINT('Ctrl Pts',(-16.7454224372302,10.9336488540573,3.90657944783047E-16));
#12964=CARTESIAN_POINT('Ctrl Pts',(-16.7512359228157,10.9192388119023,4.44089209850063E-16));
#12965=CARTESIAN_POINT('Ctrl Pts',(-16.7565956237565,10.9059535778792,4.93349777788063E-16));
#12966=CARTESIAN_POINT('Ctrl Pts',(-16.761819626096,10.8926040796307,2.41764770258606E-15));
#12967=CARTESIAN_POINT('Ctrl Pts',(-16.7668990194954,10.8792134806461,2.3037127760972E-15));
#12968=CARTESIAN_POINT('Ctrl Pts',(-16.7928605213173,10.8107722254404,1.72137516822412E-15));
#12969=CARTESIAN_POINT('Ctrl Pts',(-16.8150970458508,10.7411413575974,8.00179814752099E-16));
#12970=CARTESIAN_POINT('Ctrl Pts',(-16.8335238904444,10.6706491309863,8.32667268468867E-16));
#12971=CARTESIAN_POINT('Ctrl Pts',(-16.8518071488745,10.6007061958358,8.64901572558164E-16));
#12972=CARTESIAN_POINT('Ctrl Pts',(-16.8663399428806,10.5299142579317,1.40567801852473E-15));
#12973=CARTESIAN_POINT('Ctrl Pts',(-16.8769886640788,10.4585915479125,1.52655665885959E-15));
#12974=CARTESIAN_POINT('Ctrl Pts',(-16.8858397414576,10.3993090468971,1.6270293991195E-15));
#12975=CARTESIAN_POINT('Ctrl Pts',(-16.8920065610542,10.3396595423699,-2.49297590265314E-16));
#12976=CARTESIAN_POINT('Ctrl Pts',(-16.8953846961167,10.2798319142083,-5.82867087928207E-16));
#12977=CARTESIAN_POINT('Ctrl Pts',(-16.8967945502735,10.2548630397562,-7.22081279834834E-16));
#12978=CARTESIAN_POINT('Ctrl Pts',(-16.8977183687733,10.2298632442895,5.3650467142801E-16));
#12979=CARTESIAN_POINT('Ctrl Pts',(-16.8981472260481,10.204846807828,6.93889390390723E-16));
#12980=CARTESIAN_POINT('Ctrl Pts',(-16.8983458313901,10.1932616063874,7.66774818164271E-16));
#12981=CARTESIAN_POINT('Ctrl Pts',(-16.8984382737427,10.1816728414559,-1.02272625117412E-16));
#12982=CARTESIAN_POINT('Ctrl Pts',(-16.8984236085324,10.1700819614545,0.));
#12983=CARTESIAN_POINT('Ctrl Pts',(-16.8984083273101,10.1580042066539,1.06568585718969E-16));
#12984=CARTESIAN_POINT('Ctrl Pts',(-16.8982767333587,10.1459324667248,-2.21252032439505E-15));
#12985=CARTESIAN_POINT('Ctrl Pts',(-16.8980283738539,10.1338727649305,-2.19269047363468E-15));
#12986=CARTESIAN_POINT('Ctrl Pts',(-16.896613225799,10.0651567979331,-2.07970033559832E-15));
#12987=CARTESIAN_POINT('Ctrl Pts',(-16.8914109785722,9.9967838096264,-4.70442234551077E-16));
#12988=CARTESIAN_POINT('Ctrl Pts',(-16.8823087851953,9.92903457865317,-2.63677968348475E-16));
#12989=CARTESIAN_POINT('Ctrl Pts',(-16.8740559966144,9.86760761741545,-7.62086733775636E-17));
#12990=CARTESIAN_POINT('Ctrl Pts',(-16.8625966295214,9.80669302774072,1.74687322657192E-15));
#12991=CARTESIAN_POINT('Ctrl Pts',(-16.847811318262,9.74651168233438,1.66533453693773E-15));
#12992=CARTESIAN_POINT('Ctrl Pts',(-16.8303245125967,9.67533431762835,1.57054602216588E-15));
#12993=CARTESIAN_POINT('Ctrl Pts',(-16.8081852066777,9.60518099567779,-6.91253892319818E-16));
#12994=CARTESIAN_POINT('Ctrl Pts',(-16.7816450379385,9.53640078021501,-1.22124532708767E-15));
#12995=CARTESIAN_POINT('Ctrl Pts',(-16.7758006405534,9.52125472310633,-1.33795447788192E-15));
#12996=CARTESIAN_POINT('Ctrl Pts',(-16.7697426691712,9.50617542201614,2.209254994723E-16));
#12997=CARTESIAN_POINT('Ctrl Pts',(-16.7634735490492,9.49116691341438,2.77555756156289E-16));
#12998=CARTESIAN_POINT('Ctrl Pts',(-16.7570178531025,9.47571173529349,3.35871390794366E-16));
#12999=CARTESIAN_POINT('Ctrl Pts',(-16.7503356078206,9.46032611170409,-3.0677869516106E-15));
#13000=CARTESIAN_POINT('Ctrl Pts',(-16.74344370592,9.44504530833083,-2.96984659087229E-15));
#13001=CARTESIAN_POINT('Ctrl Pts',(-16.715244572443,9.38252186847721,-2.56911057560626E-15));
#13002=CARTESIAN_POINT('Ctrl Pts',(-16.6835082115129,9.32166957773068,-2.6303592251713E-15));
#13003=CARTESIAN_POINT('Ctrl Pts',(-16.6484903707908,9.26274125810786,-2.22044604925031E-15));
#13004=CARTESIAN_POINT('Ctrl Pts',(-16.61347982519,9.20382521477699,-1.810618268838E-15));
#13005=CARTESIAN_POINT('Ctrl Pts',(-16.5751882924367,9.14683157157451,-1.33283324348233E-15));
#13006=CARTESIAN_POINT('Ctrl Pts',(-16.5338331823285,9.09204805026436,-8.46545056276682E-16));
#13007=CARTESIAN_POINT('Ctrl Pts',(-16.503896892843,9.05239115299845,-4.94528971504313E-16));
#13008=CARTESIAN_POINT('Ctrl Pts',(-16.4723544342098,9.01389307050919,-5.66796375334866E-16));
#13009=CARTESIAN_POINT('Ctrl Pts',(-16.4392796522632,8.97667782257107,-1.04083408558608E-16));
#13010=CARTESIAN_POINT('Ctrl Pts',(-16.4144730709346,8.94876582979876,2.42958239687017E-16));
#13011=CARTESIAN_POINT('Ctrl Pts',(-16.388804365793,8.92157570849334,-2.11364162782013E-15));
#13012=CARTESIAN_POINT('Ctrl Pts',(-16.362302977449,8.89516524900551,-2.22738494315422E-15));
#13013=CARTESIAN_POINT('Ctrl Pts',(-16.3534959930271,8.88638848220873,-2.26518430646481E-15));
#13014=CARTESIAN_POINT('Ctrl Pts',(-16.3446039340464,8.87770473382657,-1.94670993893357E-15));
#13015=CARTESIAN_POINT('Ctrl Pts',(-16.3356284481052,8.8691159861548,-2.00534033822919E-15));
#13016=CARTESIAN_POINT('Ctrl Pts',(-16.2880237162768,8.82356246043644,-2.31630783946E-15));
#13017=CARTESIAN_POINT('Ctrl Pts',(-16.2380711146439,8.78067513260799,-9.30438712188027E-16));
#13018=CARTESIAN_POINT('Ctrl Pts',(-16.1859608893929,8.7407335713535,-1.61676227961038E-15));
#13019=CARTESIAN_POINT('Ctrl Pts',(-16.1492840602602,8.71262143385326,-2.09981857212978E-15));
#13020=CARTESIAN_POINT('Ctrl Pts',(-16.1115378485653,8.6859694146933,-7.92101159662489E-16));
#13021=CARTESIAN_POINT('Ctrl Pts',(-16.0727841327849,8.66088976180095,2.77555756156289E-17));
#13022=CARTESIAN_POINT('Ctrl Pts',(-16.0603479962521,8.6528416564443,2.90849064636273E-16));
#13023=CARTESIAN_POINT('Ctrl Pts',(-16.0478063459813,8.64495451082727,-3.48235544776103E-16));
#13024=CARTESIAN_POINT('Ctrl Pts',(-16.0351667481742,8.63723571788537,-4.54497550705923E-16));
#13025=CARTESIAN_POINT('Ctrl Pts',(-15.9813224568397,8.60435390137038,-9.07170372454036E-16));
#13026=CARTESIAN_POINT('Ctrl Pts',(-15.9258103363421,8.57458864949673,-5.08306115800648E-15));
#13027=CARTESIAN_POINT('Ctrl Pts',(-15.8687982055922,8.54820932690989,-3.87710696880816E-15));
#13028=CARTESIAN_POINT('Ctrl Pts',(-15.8162032016611,8.52387379415743,-2.76458644927628E-15));
#13029=CARTESIAN_POINT('Ctrl Pts',(-15.7623310456534,8.5024200146067,1.66508848905326E-17));
#13030=CARTESIAN_POINT('Ctrl Pts',(-15.7073084503787,8.48409856643006,6.50521303491303E-16));
#13031=CARTESIAN_POINT('Ctrl Pts',(-15.6970481156835,8.4806820756329,7.77638078926068E-16));
#13032=CARTESIAN_POINT('Ctrl Pts',(-15.6867477740167,8.47737461979661,7.70550576036819E-19));
#13033=CARTESIAN_POINT('Ctrl Pts',(-15.676409110153,8.47417610875465,5.55111512312578E-17));
#13034=CARTESIAN_POINT('Ctrl Pts',(-13.3882904778579,9.57816067485776,0.));
#13035=CARTESIAN_POINT('Ctrl Pts',(-13.3657943888576,9.63593729153216,-1.35606369860236E-16));
#13036=CARTESIAN_POINT('Ctrl Pts',(-13.3468720478727,9.69484378534804,4.93527622464658E-16));
#13037=CARTESIAN_POINT('Ctrl Pts',(-13.3313727466823,9.75456994412679,8.32667268468867E-17));
#13038=CARTESIAN_POINT('Ctrl Pts',(-13.3148520480641,9.81823203164207,-3.54030189194023E-16));
#13039=CARTESIAN_POINT('Ctrl Pts',(-13.3022198569086,9.88282590030355,1.2868821931612E-15));
#13040=CARTESIAN_POINT('Ctrl Pts',(-13.2933433599697,9.94801266163332,2.44249065417534E-15));
#13041=CARTESIAN_POINT('Ctrl Pts',(-13.2855764251482,10.0050510777969,3.45364805756272E-15));
#13042=CARTESIAN_POINT('Ctrl Pts',(-13.2806856940185,10.0625444259155,-6.74181128899614E-16));
#13043=CARTESIAN_POINT('Ctrl Pts',(-13.2786147667243,10.1202805657223,-6.10622663543836E-16));
#13044=CARTESIAN_POINT('Ctrl Pts',(-13.2775753306189,10.1492593852438,-5.78721512847333E-16));
#13045=CARTESIAN_POINT('Ctrl Pts',(-13.2772467443753,10.1782995334297,1.05553020072304E-15));
#13046=CARTESIAN_POINT('Ctrl Pts',(-13.2776247899912,10.2073748299843,1.16573417585641E-15));
#13047=CARTESIAN_POINT('Ctrl Pts',(-13.2777972103524,10.2206355925021,1.21599638865992E-15));
#13048=CARTESIAN_POINT('Ctrl Pts',(-13.2781168265499,10.233905381765,-2.37994547501183E-15));
#13049=CARTESIAN_POINT('Ctrl Pts',(-13.2785822538993,10.2471601602663,-2.16493489801906E-15));
#13050=CARTESIAN_POINT('Ctrl Pts',(-13.2809328514967,10.3141021879349,-1.07904394987729E-15));
#13051=CARTESIAN_POINT('Ctrl Pts',(-13.2869989993311,10.3807814420985,-1.19769074053069E-15));
#13052=CARTESIAN_POINT('Ctrl Pts',(-13.2966470399663,10.4468654449278,-8.88178419700125E-16));
#13053=CARTESIAN_POINT('Ctrl Pts',(-13.306465606786,10.5141174624129,-5.73195562712684E-16));
#13054=CARTESIAN_POINT('Ctrl Pts',(-13.3199936655056,10.5807540009591,2.66789730521724E-15));
#13055=CARTESIAN_POINT('Ctrl Pts',(-13.3371416047229,10.6464404711977,2.94209101525666E-15));
#13056=CARTESIAN_POINT('Ctrl Pts',(-13.3514848727063,10.7013834374385,3.17143833289168E-15));
#13057=CARTESIAN_POINT('Ctrl Pts',(-13.3683616484046,10.755662308463,1.19948474334804E-15));
#13058=CARTESIAN_POINT('Ctrl Pts',(-13.3877471973421,10.8090815757484,9.99200722162641E-16));
#13059=CARTESIAN_POINT('Ctrl Pts',(-13.396683355205,10.8337062591617,9.06875782771859E-16));
#13060=CARTESIAN_POINT('Ctrl Pts',(-13.406152962408,10.8581482388832,2.06346452769943E-15));
#13061=CARTESIAN_POINT('Ctrl Pts',(-13.4161553992987,10.8823879424951,2.22044604925031E-15));
#13062=CARTESIAN_POINT('Ctrl Pts',(-13.4205138927756,10.892950227589,2.28884967380167E-15));
#13063=CARTESIAN_POINT('Ctrl Pts',(-13.4249735407989,10.9034737969884,6.01283625265369E-16));
#13064=CARTESIAN_POINT('Ctrl Pts',(-13.4295285164776,10.9139442825721,6.66133814775094E-16));
#13065=CARTESIAN_POINT('Ctrl Pts',(-13.4575211485423,10.9782907184605,1.06467106772917E-15));
#13066=CARTESIAN_POINT('Ctrl Pts',(-13.4891600706501,11.0407558305742,3.69548560173297E-15));
#13067=CARTESIAN_POINT('Ctrl Pts',(-13.5243384304155,11.1009910327419,3.41393580072236E-15));
#13068=CARTESIAN_POINT('Ctrl Pts',(-13.5557931413997,11.1548503055419,3.16218820141692E-15));
#13069=CARTESIAN_POINT('Ctrl Pts',(-13.5900783758293,11.2069274748198,4.73664851661874E-16));
#13070=CARTESIAN_POINT('Ctrl Pts',(-13.6271528815519,11.2569698990377,8.04911692853238E-16));
#13071=CARTESIAN_POINT('Ctrl Pts',(-13.6675377331972,11.3114805617862,1.17809376743549E-15));
#13072=CARTESIAN_POINT('Ctrl Pts',(-13.7112315791046,11.3635781179213,1.8548613205985E-15));
#13073=CARTESIAN_POINT('Ctrl Pts',(-13.7579205122475,11.4131764577819,1.84574577843932E-15));
#13074=CARTESIAN_POINT('Ctrl Pts',(-13.7759296243692,11.432307802267,1.84222968137425E-15));
#13075=CARTESIAN_POINT('Ctrl Pts',(-13.7943848362944,11.4510670204427,2.04120230226521E-16));
#13076=CARTESIAN_POINT('Ctrl Pts',(-13.8132698004889,11.4694480131946,-1.38777878078145E-17));
#13077=CARTESIAN_POINT('Ctrl Pts',(-13.8215554419107,11.4775125407918,-1.09522841168832E-16));
#13078=CARTESIAN_POINT('Ctrl Pts',(-13.8299234502305,11.485503775114,4.05044125615248E-15));
#13079=CARTESIAN_POINT('Ctrl Pts',(-13.8383624555639,11.4934121444084,3.92741394961149E-15));
#13080=CARTESIAN_POINT('Ctrl Pts',(-13.8893881936728,11.5412294362029,3.18353965687582E-15));
#13081=CARTESIAN_POINT('Ctrl Pts',(-13.9430957557082,11.586107963496,3.38934266541307E-15));
#13082=CARTESIAN_POINT('Ctrl Pts',(-13.9991081910456,11.6279861648249,3.09474668114262E-15));
#13083=CARTESIAN_POINT('Ctrl Pts',(-14.0564205721683,11.6708362823183,2.7933136649555E-15));
#13084=CARTESIAN_POINT('Ctrl Pts',(-14.1161466797624,11.7105458009547,1.50938421367961E-15));
#13085=CARTESIAN_POINT('Ctrl Pts',(-14.1779316897435,11.747021082115,1.41553435639707E-15));
#13086=CARTESIAN_POINT('Ctrl Pts',(-14.2252011257199,11.7749269765716,1.34373328650058E-15));
#13087=CARTESIAN_POINT('Ctrl Pts',(-14.2736767913047,11.8009393030142,-9.76164430457898E-17));
#13088=CARTESIAN_POINT('Ctrl Pts',(-14.3232147340873,11.8250021795641,-4.37150315946155E-16));
#13089=CARTESIAN_POINT('Ctrl Pts',(-14.3540404755327,11.8399756719881,-6.48430453756458E-16));
#13090=CARTESIAN_POINT('Ctrl Pts',(-14.3852777833939,11.8541940595482,2.95554805743735E-15));
#13091=CARTESIAN_POINT('Ctrl Pts',(-14.4168938523755,11.8676411051472,3.06005221162309E-15));
#13092=CARTESIAN_POINT('Ctrl Pts',(-14.4346635095532,11.875198951459,3.11878826114919E-15));
#13093=CARTESIAN_POINT('Ctrl Pts',(-14.4525588814166,11.8825153089168,3.62295386493415E-15));
#13094=CARTESIAN_POINT('Ctrl Pts',(-14.4705415223192,11.889574578414,3.62210261783957E-15));
#13095=CARTESIAN_POINT('Ctrl Pts',(-14.5401794861377,11.9169116729204,3.61880615461739E-15));
#13096=CARTESIAN_POINT('Ctrl Pts',(-14.6111927842436,11.9404289151015,2.34519441392117E-15));
#13097=CARTESIAN_POINT('Ctrl Pts',(-14.6832097355402,11.9600120506473,2.49106291150269E-15));
#13098=CARTESIAN_POINT('Ctrl Pts',(-14.7370845061574,11.9746618923373,2.60018488495465E-15));
#13099=CARTESIAN_POINT('Ctrl Pts',(-14.7915219084323,11.9871094077609,9.59298669237085E-16));
#13100=CARTESIAN_POINT('Ctrl Pts',(-14.8463768906533,11.9972908526876,5.30825383648903E-16));
#13101=CARTESIAN_POINT('Ctrl Pts',(-14.8634609542423,12.0004617670789,3.97381445453818E-16));
#13102=CARTESIAN_POINT('Ctrl Pts',(-14.8805855708211,12.0034127746477,-1.21629321462611E-15));
#13103=CARTESIAN_POINT('Ctrl Pts',(-14.8977464763661,12.0061416440875,-1.23165366794353E-15));
#13104=CARTESIAN_POINT('Ctrl Pts',(-14.9143450435635,12.008781092376,-1.24651078115971E-15));
#13105=CARTESIAN_POINT('Ctrl Pts',(-14.9309691166948,12.0112113262329,1.37759135887431E-15));
#13106=CARTESIAN_POINT('Ctrl Pts',(-14.9476086885424,12.0134301728835,1.19002030452009E-15));
#13107=CARTESIAN_POINT('Ctrl Pts',(-15.0222847381472,12.0233880434379,3.48227890169128E-16));
#13108=CARTESIAN_POINT('Ctrl Pts',(-15.0973088346763,12.0290980641533,1.29347754135401E-16));
#13109=CARTESIAN_POINT('Ctrl Pts',(-15.1723239977792,12.0304219868111,1.2195106036117E-15));
#13110=CARTESIAN_POINT('Ctrl Pts',(-15.2297783091666,12.0314359826685,2.05446920699172E-15));
#13111=CARTESIAN_POINT('Ctrl Pts',(-15.2872280829805,12.029876276423,1.66503248027151E-15));
#13112=CARTESIAN_POINT('Ctrl Pts',(-15.3445188409063,12.0256608695019,1.6605640473788E-15));
#13113=CARTESIAN_POINT('Ctrl Pts',(-15.3577646096558,12.0246862567147,1.64941776864115E-15));
#13114=CARTESIAN_POINT('Ctrl Pts',(-15.371001888815,12.0235696055055,1.03965794060541E-15));
#13115=CARTESIAN_POINT('Ctrl Pts',(-15.384229221931,12.022312258029,1.0547118733939E-15));
#13116=CARTESIAN_POINT('Ctrl Pts',(13.6609982804014,11.5585480285869,0.));
#13117=CARTESIAN_POINT('Ctrl Pts',(13.6101587848434,11.505843297701,1.58535375005519E-16));
#13118=CARTESIAN_POINT('Ctrl Pts',(13.562541153526,11.4503742643279,2.04729506994165E-15));
#13119=CARTESIAN_POINT('Ctrl Pts',(13.5181883216384,11.3924875417427,2.02615701994091E-15));
#13120=CARTESIAN_POINT('Ctrl Pts',(13.4726057261298,11.3329958035915,2.00443287873015E-15));
#13121=CARTESIAN_POINT('Ctrl Pts',(13.4304710888115,11.2709494929059,-1.04515563626232E-15));
#13122=CARTESIAN_POINT('Ctrl Pts',(13.3918785046867,11.2066981958572,-9.99200722162641E-16));
#13123=CARTESIAN_POINT('Ctrl Pts',(13.359268347745,11.1524068098827,-9.60369506398756E-16));
#13124=CARTESIAN_POINT('Ctrl Pts',(13.329187972469,11.0965402628436,1.19891982664628E-15));
#13125=CARTESIAN_POINT('Ctrl Pts',(13.3017224576139,11.0393031054692,2.05391259555654E-15));
#13126=CARTESIAN_POINT('Ctrl Pts',(13.2895238929487,11.0138817300036,2.43365004577085E-15));
#13127=CARTESIAN_POINT('Ctrl Pts',(13.2778414898473,10.9881899564878,1.38699052202662E-15));
#13128=CARTESIAN_POINT('Ctrl Pts',(13.2666844138171,10.9622457275511,1.36002320516582E-15));
#13129=CARTESIAN_POINT('Ctrl Pts',(13.2605518218175,10.9479852375819,1.34520036527618E-15));
#13130=CARTESIAN_POINT('Ctrl Pts',(13.2545779632859,10.9336484761084,3.15224287654931E-15));
#13131=CARTESIAN_POINT('Ctrl Pts',(13.2487644993064,10.9192384434638,3.1641356201817E-15));
#13132=CARTESIAN_POINT('Ctrl Pts',(13.2434047935862,10.9059531569865,3.17510009958671E-15));
#13133=CARTESIAN_POINT('Ctrl Pts',(13.2381807873077,10.8926036056845,3.12885909062377E-16));
#13134=CARTESIAN_POINT('Ctrl Pts',(13.2331013908405,10.8792129532788,3.33066907387547E-16));
#13135=CARTESIAN_POINT('Ctrl Pts',(13.2071399443245,10.8107716121686,4.36214577006048E-16));
#13136=CARTESIAN_POINT('Ctrl Pts',(13.1849034774407,10.7411406550117,-1.22541225100052E-15));
#13137=CARTESIAN_POINT('Ctrl Pts',(13.1664766897913,10.6706483399882,-1.08246744900953E-15));
#13138=CARTESIAN_POINT('Ctrl Pts',(13.1481934814117,10.6007052924391,-9.40636455386775E-16));
#13139=CARTESIAN_POINT('Ctrl Pts',(13.1336607394114,10.5299132424147,1.19000295853796E-15));
#13140=CARTESIAN_POINT('Ctrl Pts',(13.1230120693126,10.4585904251542,1.11022302462516E-15));
#13141=CARTESIAN_POINT('Ctrl Pts',(13.1141610384968,10.399307862394,1.04391102068517E-15));
#13142=CARTESIAN_POINT('Ctrl Pts',(13.1079942623606,10.3396582998303,-8.10480048155446E-17));
#13143=CARTESIAN_POINT('Ctrl Pts',(13.1046161658339,10.2798306198277,0.));
#13144=CARTESIAN_POINT('Ctrl Pts',(13.1032063285254,10.2548617372976,3.38251142524164E-17));
#13145=CARTESIAN_POINT('Ctrl Pts',(13.1022825254872,10.229861934867,7.93924619007334E-16));
#13146=CARTESIAN_POINT('Ctrl Pts',(13.1018536821348,10.2048454927203,5.82867087928207E-16));
#13147=CARTESIAN_POINT('Ctrl Pts',(13.1016550834447,10.1932603005737,4.85125689003432E-16));
#13148=CARTESIAN_POINT('Ctrl Pts',(13.1015626471952,10.1816715452178,3.96242804970713E-16));
#13149=CARTESIAN_POINT('Ctrl Pts',(13.1015773179414,10.1700806750858,3.33066907387547E-16));
#13150=CARTESIAN_POINT('Ctrl Pts',(13.1015926049752,10.1580028966096,2.67237121758476E-16));
#13151=CARTESIAN_POINT('Ctrl Pts',(13.1017242047727,10.1459311332672,2.51600957460125E-15));
#13152=CARTESIAN_POINT('Ctrl Pts',(13.1019725701435,10.1338714084625,2.44249065417534E-15));
#13153=CARTESIAN_POINT('Ctrl Pts',(13.1033877505433,10.06515536275,2.02358146855792E-15));
#13154=CARTESIAN_POINT('Ctrl Pts',(13.1085900250014,9.99678230711821,1.45205686412796E-15));
#13155=CARTESIAN_POINT('Ctrl Pts',(13.1176922379213,9.92903302435398,1.04083408558608E-15));
#13156=CARTESIAN_POINT('Ctrl Pts',(13.1259450381762,9.86760606115364,6.67986352680291E-16));
#13157=CARTESIAN_POINT('Ctrl Pts',(13.1374044059322,9.80669148153412,4.49301831864335E-16));
#13158=CARTESIAN_POINT('Ctrl Pts',(13.152189704592,9.74651016097886,5.27355936696949E-16));
#13159=CARTESIAN_POINT('Ctrl Pts',(13.1696765010495,9.67533280248825,6.06618167751903E-16));
#13160=CARTESIAN_POINT('Ctrl Pts',(13.1918157822245,9.60517950813245,1.45195337725464E-15));
#13161=CARTESIAN_POINT('Ctrl Pts',(13.2183559139599,9.5363993371827,1.48492329543615E-15));
#13162=CARTESIAN_POINT('Ctrl Pts',(13.2242003063607,9.5212532816756,1.49218358868559E-15));
#13163=CARTESIAN_POINT('Ctrl Pts',(13.2302582723953,9.50617398307989,1.82761809169572E-15));
#13164=CARTESIAN_POINT('Ctrl Pts',(13.2365273868373,9.49116547782453,1.97064586870965E-15));
#13165=CARTESIAN_POINT('Ctrl Pts',(13.2429830702302,9.47571031920141,2.11793015476297E-15));
#13166=CARTESIAN_POINT('Ctrl Pts',(13.2496653021317,9.46032471587291,-4.47659329837229E-17));
#13167=CARTESIAN_POINT('Ctrl Pts',(13.2565571899036,9.44504393340732,8.32667268468867E-17));
#13168=CARTESIAN_POINT('Ctrl Pts',(13.2847562783215,9.38252055082999,6.07129623986592E-16));
#13169=CARTESIAN_POINT('Ctrl Pts',(13.316492584851,9.32166832971813,1.1675802761368E-15));
#13170=CARTESIAN_POINT('Ctrl Pts',(13.3515103647051,9.26274008818287,1.11022302462516E-15));
#13171=CARTESIAN_POINT('Ctrl Pts',(13.3865208536858,9.20382411579612,1.0528777151742E-15));
#13172=CARTESIAN_POINT('Ctrl Pts',(13.4248123241401,9.1468305524612,1.81328320611437E-15));
#13173=CARTESIAN_POINT('Ctrl Pts',(13.4661673690105,9.09204711620811,1.52655665885959E-15));
#13174=CARTESIAN_POINT('Ctrl Pts',(13.4961036636995,9.05239021106192,1.31899962583875E-15));
#13175=CARTESIAN_POINT('Ctrl Pts',(13.5276461316194,9.01389212746855,1.12431972020032E-15));
#13176=CARTESIAN_POINT('Ctrl Pts',(13.5607209276105,8.97667688443461,1.38777878078145E-15));
#13177=CARTESIAN_POINT('Ctrl Pts',(13.585527516553,8.94876489862573,1.58537699486414E-15));
#13178=CARTESIAN_POINT('Ctrl Pts',(13.6111962317832,8.92157478749522,9.51776285385933E-16));
#13179=CARTESIAN_POINT('Ctrl Pts',(13.637697633009,8.89516434107376,1.29757316003065E-15));
#13180=CARTESIAN_POINT('Ctrl Pts',(13.6465045264423,8.88638767356186,1.41248769600548E-15));
#13181=CARTESIAN_POINT('Ctrl Pts',(13.655396492531,8.87770402312783,3.58625279291791E-15));
#13182=CARTESIAN_POINT('Ctrl Pts',(13.6643718842665,8.86911537146476,3.39311911901063E-15));
#13183=CARTESIAN_POINT('Ctrl Pts',(13.7119765765409,8.82356191468833,2.3687550148941E-15));
#13184=CARTESIAN_POINT('Ctrl Pts',(13.7619291420876,8.78067465781436,8.91728926236411E-16));
#13185=CARTESIAN_POINT('Ctrl Pts',(13.8140393370137,8.7407331665078,1.15879528195251E-15));
#13186=CARTESIAN_POINT('Ctrl Pts',(13.8507161652704,8.71262106255111,1.34676515762891E-15));
#13187=CARTESIAN_POINT('Ctrl Pts',(13.8884623801383,8.68596907806574,4.57265468878883E-16));
#13188=CARTESIAN_POINT('Ctrl Pts',(13.9272161038781,8.66088946010809,6.21031004399697E-16));
#13189=CARTESIAN_POINT('Ctrl Pts',(13.9396522240711,8.65284137818927,6.73583577073472E-16));
#13190=CARTESIAN_POINT('Ctrl Pts',(13.9521938582917,8.64495425547895,-6.90481307027163E-16));
#13191=CARTESIAN_POINT('Ctrl Pts',(13.9648334399852,8.63723548509471,-4.78783679369599E-16));
#13192=CARTESIAN_POINT('Ctrl Pts',(14.0186777326348,8.60435372195212,4.23042764994196E-16));
#13193=CARTESIAN_POINT('Ctrl Pts',(14.0741898629058,8.57458852180253,1.67668390097511E-15));
#13194=CARTESIAN_POINT('Ctrl Pts',(14.1312020138798,8.54820924684521,9.10729824887824E-16));
#13195=CARTESIAN_POINT('Ctrl Pts',(14.1837968242759,8.52387385621248,2.04122396196814E-16));
#13196=CARTESIAN_POINT('Ctrl Pts',(14.237668785338,8.50242019207491,4.24437901475045E-16));
#13197=CARTESIAN_POINT('Ctrl Pts',(14.292691187472,8.48409882756164,7.38124839028131E-16));
#13198=CARTESIAN_POINT('Ctrl Pts',(14.3029515183617,8.48068234164015,8.02378731734645E-16));
#13199=CARTESIAN_POINT('Ctrl Pts',(14.3132518565374,8.47737489025808,-2.18489316463771E-17));
#13200=CARTESIAN_POINT('Ctrl Pts',(14.3235905172155,8.47417638326182,1.38777878078145E-17));
#13201=CARTESIAN_POINT('Ctrl Pts',(16.6117095221421,9.57816067485776,0.));
#13202=CARTESIAN_POINT('Ctrl Pts',(16.6342056260937,9.63593732993143,-5.64453285222628E-17));
#13203=CARTESIAN_POINT('Ctrl Pts',(16.6531279845489,9.69484386095271,2.56255980870842E-15));
#13204=CARTESIAN_POINT('Ctrl Pts',(16.6686273043538,9.75457005573485,2.22044604925031E-15));
#13205=CARTESIAN_POINT('Ctrl Pts',(16.6851480105456,9.8182321343534,1.85578740775209E-15));
#13206=CARTESIAN_POINT('Ctrl Pts',(16.6977802163463,9.88282599137373,2.5349006953864E-16));
#13207=CARTESIAN_POINT('Ctrl Pts',(16.7066567330792,9.94801273908534,1.0547118733939E-15));
#13208=CARTESIAN_POINT('Ctrl Pts',(16.7144236852204,10.005051143333,1.75578095176725E-15));
#13209=CARTESIAN_POINT('Ctrl Pts',(16.719314437616,10.0625444780201,6.09173409191634E-16));
#13210=CARTESIAN_POINT('Ctrl Pts',(16.7213853889065,10.1202806033607,2.22044604925031E-16));
#13211=CARTESIAN_POINT('Ctrl Pts',(16.722424837962,10.1492594408788,2.77374419265692E-17));
#13212=CARTESIAN_POINT('Ctrl Pts',(16.7227534366055,10.1782996069071,1.90884567343023E-15));
#13213=CARTESIAN_POINT('Ctrl Pts',(16.7223754026995,10.2073749211407,2.22044604925031E-15));
#13214=CARTESIAN_POINT('Ctrl Pts',(16.7222029883378,10.2206356410525,2.36256129089315E-15));
#13215=CARTESIAN_POINT('Ctrl Pts',(16.7218833791234,10.2339053875377,5.13100323005786E-16));
#13216=CARTESIAN_POINT('Ctrl Pts',(16.7214179597069,10.247160123306,5.27355936696949E-16));
#13217=CARTESIAN_POINT('Ctrl Pts',(16.7190673940356,10.3141021669321,5.99352838808771E-16));
#13218=CARTESIAN_POINT('Ctrl Pts',(16.7130012766232,10.3807814360522,-1.43723603342314E-15));
#13219=CARTESIAN_POINT('Ctrl Pts',(16.7033532632529,10.446865453063,-1.22124532708767E-15));
#13220=CARTESIAN_POINT('Ctrl Pts',(16.6935347267057,10.5141174676801,-1.00143710723863E-15));
#13221=CARTESIAN_POINT('Ctrl Pts',(16.6800066968994,10.5807540028731,2.94558620309747E-15));
#13222=CARTESIAN_POINT('Ctrl Pts',(16.6628587834113,10.6464404697601,3.63598040564739E-15));
#13223=CARTESIAN_POINT('Ctrl Pts',(16.6485155430073,10.7013834099898,4.21345532861642E-15));
#13224=CARTESIAN_POINT('Ctrl Pts',(16.6316387948011,10.7556622555645,8.18121107440506E-16));
#13225=CARTESIAN_POINT('Ctrl Pts',(16.6122532721583,10.8090814984855,4.44089209850063E-16));
#13226=CARTESIAN_POINT('Ctrl Pts',(16.6033171160797,10.8337061991522,2.71671500158053E-16));
#13227=CARTESIAN_POINT('Ctrl Pts',(16.5938475091728,10.8581481959351,1.39602086560423E-15));
#13228=CARTESIAN_POINT('Ctrl Pts',(16.5838450709829,10.8823879164002,1.41553435639707E-15));
#13229=CARTESIAN_POINT('Ctrl Pts',(16.5794865922092,10.8929501718345,1.42403719678521E-15));
#13230=CARTESIAN_POINT('Ctrl Pts',(16.5750269593375,10.9034737117046,1.48442318111539E-15));
#13231=CARTESIAN_POINT('Ctrl Pts',(16.570471999173,10.9139441680789,1.52655665885959E-15));
#13232=CARTESIAN_POINT('Ctrl Pts',(16.5424793917532,10.9782905869741,1.78548886883269E-15));
#13233=CARTESIAN_POINT('Ctrl Pts',(16.5108404898856,11.0407556838492,-1.7236150121703E-16));
#13234=CARTESIAN_POINT('Ctrl Pts',(16.4756621440164,11.100990873284,0.));
#13235=CARTESIAN_POINT('Ctrl Pts',(16.444207459148,11.1548501112569,1.54116874181183E-16));
#13236=CARTESIAN_POINT('Ctrl Pts',(16.409922248227,11.2069272492601,1.27367449426832E-15));
#13237=CARTESIAN_POINT('Ctrl Pts',(16.3728477619717,11.2569696466227,6.38378239159465E-16));
#13238=CARTESIAN_POINT('Ctrl Pts',(16.3324629238938,11.3114802904279,-5.21238641377393E-17));
#13239=CARTESIAN_POINT('Ctrl Pts',(16.2887690855124,11.3635778319471,2.57197908009856E-15));
#13240=CARTESIAN_POINT('Ctrl Pts',(16.2420801551,11.4131761610744,2.05391259555654E-15));
#13241=CARTESIAN_POINT('Ctrl Pts',(16.2240710321118,11.4323075140818,1.85408100905903E-15));
#13242=CARTESIAN_POINT('Ctrl Pts',(16.2056158080157,11.4510667408658,4.27898362178755E-16));
#13243=CARTESIAN_POINT('Ctrl Pts',(16.186730830448,11.4694477422767,1.38777878078145E-17));
#13244=CARTESIAN_POINT('Ctrl Pts',(16.1784451837245,11.4775122731223,-1.6777073166606E-16));
#13245=CARTESIAN_POINT('Ctrl Pts',(16.1700771698675,11.4855035107274,2.9199856936581E-15));
#13246=CARTESIAN_POINT('Ctrl Pts',(16.1616381587957,11.4934118833135,2.92821322744885E-15));
#13247=CARTESIAN_POINT('Ctrl Pts',(16.1106124187267,11.5412291643329,2.97796028869198E-15));
#13248=CARTESIAN_POINT('Ctrl Pts',(16.0569048507137,11.5861076850411,4.00406114414307E-15));
#13249=CARTESIAN_POINT('Ctrl Pts',(16.0008924066742,11.627985883466,3.77475828372553E-15));
#13250=CARTESIAN_POINT('Ctrl Pts',(15.9435800064801,11.6708360055897,3.54013368329494E-15));
#13251=CARTESIAN_POINT('Ctrl Pts',(15.8838538761052,11.7105455315968,2.16385081713861E-15));
#13252=CARTESIAN_POINT('Ctrl Pts',(15.8220688411562,11.7470208223532,1.04083408558608E-15));
#13253=CARTESIAN_POINT('Ctrl Pts',(15.7747993280594,11.7749267584029,1.81654283488492E-16));
#13254=CARTESIAN_POINT('Ctrl Pts',(15.726323581113,11.8009391230971,2.17035692847852E-15));
#13255=CARTESIAN_POINT('Ctrl Pts',(15.6767855539149,11.825002034133,1.99146255042137E-15));
#13256=CARTESIAN_POINT('Ctrl Pts',(15.6459597802179,11.839975538167,1.88014286480683E-15));
#13257=CARTESIAN_POINT('Ctrl Pts',(15.6147224394625,11.8541939368713,2.96650020135072E-15));
#13258=CARTESIAN_POINT('Ctrl Pts',(15.5831063371564,11.8676409930684,3.44169137633799E-15));
#13259=CARTESIAN_POINT('Ctrl Pts',(15.5653366958438,11.8751988306228,3.70876973573554E-15));
#13260=CARTESIAN_POINT('Ctrl Pts',(15.5474413401978,11.882515180091,1.95911521127522E-15));
#13261=CARTESIAN_POINT('Ctrl Pts',(15.5294587157909,11.8895744424011,1.99146255042137E-15));
#13262=CARTESIAN_POINT('Ctrl Pts',(15.4598207086011,11.916911551178,2.11672815042826E-15));
#13263=CARTESIAN_POINT('Ctrl Pts',(15.3888073670723,11.9404288078564,3.08329528087669E-15));
#13264=CARTESIAN_POINT('Ctrl Pts',(15.3167903740727,11.9600119575184,2.22044604925031E-15));
#13265=CARTESIAN_POINT('Ctrl Pts',(15.2629155692888,11.9746618105761,1.57496181038276E-15));
#13266=CARTESIAN_POINT('Ctrl Pts',(15.2084781337459,11.9871093369122,5.48219519405437E-16));
#13267=CARTESIAN_POINT('Ctrl Pts',(15.1536231199128,11.9972907920356,4.82253126321552E-16));
#13268=CARTESIAN_POINT('Ctrl Pts',(15.1365390543032,12.0004617081502,4.61708528686322E-16));
#13269=CARTESIAN_POINT('Ctrl Pts',(15.1194144359014,12.0034127175744,2.83080269845694E-15));
#13270=CARTESIAN_POINT('Ctrl Pts',(15.1022535287486,12.0061415889966,3.01147995429574E-15));
#13271=CARTESIAN_POINT('Ctrl Pts',(15.0856549463322,12.0087810413753,3.18623681855123E-15));
#13272=CARTESIAN_POINT('Ctrl Pts',(15.0690308581054,12.0112112791014,-3.4217463351498E-16));
#13273=CARTESIAN_POINT('Ctrl Pts',(15.0523912713646,12.0134301293824,-4.19803081186387E-16));
#13274=CARTESIAN_POINT('Ctrl Pts',(14.977715184966,12.0233880122238,-7.68188456112627E-16));
#13275=CARTESIAN_POINT('Ctrl Pts',(14.9026910556725,12.0290980438973,1.15979021628154E-15));
#13276=CARTESIAN_POINT('Ctrl Pts',(14.8276758656066,12.0304219755773,1.86656246015104E-15));
#13277=CARTESIAN_POINT('Ctrl Pts',(14.7702215268349,12.0314359784637,2.40788125035953E-15));
#13278=CARTESIAN_POINT('Ctrl Pts',(14.7127717290399,12.0298762775092,7.42876097831855E-16));
#13279=CARTESIAN_POINT('Ctrl Pts',(14.655480951399,12.0256608738343,-1.99493199737333E-17));
#13280=CARTESIAN_POINT('Ctrl Pts',(14.642235179624,12.0246862619105,-1.99785920673064E-16));
#13281=CARTESIAN_POINT('Ctrl Pts',(14.6289978976654,12.0235696114882,1.00718411817654E-15));
#13282=CARTESIAN_POINT('Ctrl Pts',(14.6157705619694,12.0223122647246,1.04083408558608E-15));
#13283=CARTESIAN_POINT('Origin',(15.,10.,9.54592528053767));
#13284=CARTESIAN_POINT('Ctrl Pts',(12.9434528818545,10.0014882284141,7.79592528053768));
#13285=CARTESIAN_POINT('Ctrl Pts',(12.9426313256354,10.0998548223026,7.79057696270225));
#13286=CARTESIAN_POINT('Ctrl Pts',(12.9937604030143,10.8787658748103,7.74818159569048));
#13287=CARTESIAN_POINT('Ctrl Pts',(13.989390948843,12.2086082123096,7.66873917950236));
#13288=CARTESIAN_POINT('Ctrl Pts',(16.3073490337982,12.0466292797422,7.55759803197335));
#13289=CARTESIAN_POINT('Ctrl Pts',(17.4286195856453,10.0116469634969,7.44645688444433));
#13290=CARTESIAN_POINT('Ctrl Pts',(16.3268236193488,7.9657970755479,7.33531573691531));
#13291=CARTESIAN_POINT('Ctrl Pts',(14.0105079180419,7.78208259180166,7.22417458938629));
#13292=CARTESIAN_POINT('Ctrl Pts',(12.9977472036765,9.10777343312236,7.14437777059375));
#13293=CARTESIAN_POINT('Ctrl Pts',(12.9427343174564,9.89346179907822,7.10162800097754));
#13294=CARTESIAN_POINT('Ctrl Pts',(12.9436341942584,9.99839713117394,7.09592528053768));
#13295=CARTESIAN_POINT('Ctrl Pts',(12.9473113968994,9.99752941021421,7.85407471946233));
#13296=CARTESIAN_POINT('Ctrl Pts',(12.9508756442256,10.4678337643571,7.82862238128887));
#13297=CARTESIAN_POINT('Ctrl Pts',(13.3435591556684,11.6297989150585,7.76612299393907));
#13298=CARTESIAN_POINT('Ctrl Pts',(15.2723377259255,12.4126882042673,7.66657655741295));
#13299=CARTESIAN_POINT('Ctrl Pts',(17.1748665662283,11.0807510628696,7.55543540988391));
#13300=CARTESIAN_POINT('Ctrl Pts',(17.0874397300721,8.75827685188236,7.44429426235491));
#13301=CARTESIAN_POINT('Ctrl Pts',(15.0888245216199,7.57307606901691,7.33315311482588));
#13302=CARTESIAN_POINT('Ctrl Pts',(13.2786046599163,8.4748124919398,7.23641326719502));
#13303=CARTESIAN_POINT('Ctrl Pts',(12.9501053395568,9.58221924013019,7.1767204687405));
#13304=CARTESIAN_POINT('Ctrl Pts',(12.9479405474349,10.0011587877502,7.15407471946232));
#13305=CARTESIAN_POINT('Ctrl Pts',(16.2690708798524,11.0793586530485,8.));
#13306=CARTESIAN_POINT('Ctrl Pts',(16.6279938291456,10.657350026192,7.96295295082366));
#13307=CARTESIAN_POINT('Ctrl Pts',(16.8854598801969,9.43433251832768,7.88885885247098));
#13308=CARTESIAN_POINT('Ctrl Pts',(15.5448845996416,8.10642602073482,7.77771770494196));
#13309=CARTESIAN_POINT('Ctrl Pts',(13.7057107168279,8.51663622362914,7.66657655741294));
#13310=CARTESIAN_POINT('Ctrl Pts',(13.0512228488578,10.282272228723,7.55543540988393));
#13311=CARTESIAN_POINT('Ctrl Pts',(14.1805939023105,11.7907488899904,7.4442942623549));
#13312=CARTESIAN_POINT('Ctrl Pts',(16.0600041320393,11.6594156856311,7.33315311482588));
#13313=CARTESIAN_POINT('Ctrl Pts',(16.9691350430393,10.0094434073176,7.22201196729686));
#13314=CARTESIAN_POINT('Ctrl Pts',(16.075794208461,8.35065965585243,7.11087081976784));
#13315=CARTESIAN_POINT('Ctrl Pts',(14.1977156303481,8.20170317456703,6.99972967223882));
#13316=CARTESIAN_POINT('Ctrl Pts',(13.0540155464189,9.69879197844384,6.8885885247098));
#13317=CARTESIAN_POINT('Ctrl Pts',(13.6915931588825,11.4716176684,6.77744737718079));
#13318=CARTESIAN_POINT('Ctrl Pts',(15.5268344256012,11.8973708763893,6.66630622965175));
#13319=CARTESIAN_POINT('Ctrl Pts',(16.8798324113308,10.5863519109992,6.55516508212275));
#13320=CARTESIAN_POINT('Ctrl Pts',(16.5121060647823,8.73860643490976,6.44402393459371));
#13321=CARTESIAN_POINT('Ctrl Pts',(14.7602576417037,8.04549238469812,6.33288278706472));
#13322=CARTESIAN_POINT('Ctrl Pts',(13.2278598780647,9.14145649340251,6.22174163953567));
#13323=CARTESIAN_POINT('Ctrl Pts',(13.3176091277843,11.0232978176747,6.11060049200667));
#13324=CARTESIAN_POINT('Ctrl Pts',(14.9473524627353,11.9684525532754,5.99945934447763));
#13325=CARTESIAN_POINT('Ctrl Pts',(16.6252872741601,11.1117637611562,5.88831819694864));
#13326=CARTESIAN_POINT('Ctrl Pts',(16.8154983706705,9.23741031714155,5.7771770494196));
#13327=CARTESIAN_POINT('Ctrl Pts',(15.3438740364888,8.06110134986314,5.66603590189059));
#13328=CARTESIAN_POINT('Ctrl Pts',(13.5574810043252,8.65958353517834,5.55489475436156));
#13329=CARTESIAN_POINT('Ctrl Pts',(13.091512829808,10.4850299660946,5.44375360683254));
#13330=CARTESIAN_POINT('Ctrl Pts',(14.372498357211,11.866499137894,5.33261245930353));
#13331=CARTESIAN_POINT('Ctrl Pts',(16.2278740796803,11.5394487945932,5.22147131177451));
#13332=CARTESIAN_POINT('Ctrl Pts',(16.9593024145856,9.80324788695935,5.11033016424548));
#13333=CARTESIAN_POINT('Ctrl Pts',(15.8972627818015,8.24714608542604,4.99918901671647));
#13334=CARTESIAN_POINT('Ctrl Pts',(14.0139042725623,8.29553745649413,4.88804786918744));
#13335=CARTESIAN_POINT('Ctrl Pts',(13.0331788061281,9.90412645273168,4.77690672165843));
#13336=CARTESIAN_POINT('Ctrl Pts',(13.852803700691,11.6004743036209,4.6657655741294));
#13337=CARTESIAN_POINT('Ctrl Pts',(15.7225267323057,11.8318112530665,4.55462442660039));
#13338=CARTESIAN_POINT('Ctrl Pts',(16.9308773588479,10.3863806035781,4.44348327907136));
#13339=CARTESIAN_POINT('Ctrl Pts',(16.3717791899039,8.58727242545577,4.33234213154234));
#13340=CARTESIAN_POINT('Ctrl Pts',(14.557008584925,8.08131921573479,4.22120098401333));
#13341=CARTESIAN_POINT('Ctrl Pts',(13.1477348072808,9.33165053933164,4.1100598364843));
#13342=CARTESIAN_POINT('Ctrl Pts',(13.4339513562445,11.1937625354845,3.99891868895529));
#13343=CARTESIAN_POINT('Ctrl Pts',(15.1536669186984,11.9631515030262,3.88777754142627));
#13344=CARTESIAN_POINT('Ctrl Pts',(16.7327218591219,10.9355491994844,3.77663639389724));
#13345=CARTESIAN_POINT('Ctrl Pts',(16.72571171427,9.0515821464321,3.66549524636823));
#13346=CARTESIAN_POINT('Ctrl Pts',(15.1390532935877,8.03575930006501,3.5543540988392));
#13347=CARTESIAN_POINT('Ctrl Pts',(13.4251109855405,8.81792473257162,3.44321295131019));
#13348=CARTESIAN_POINT('Ctrl Pts',(13.1527598168138,10.6821151305718,3.33207180378117));
#13349=CARTESIAN_POINT('Ctrl Pts',(14.5712992796378,11.9219243060325,3.22093065625215));
#13350=CARTESIAN_POINT('Ctrl Pts',(16.3822544328478,11.4024799565668,3.10978950872313));
#13351=CARTESIAN_POINT('Ctrl Pts',(16.9279485267848,9.5992609030834,2.99864836119411));
#13352=CARTESIAN_POINT('Ctrl Pts',(15.7088747623015,8.1628625752935,2.88750721366509));
#13353=CARTESIAN_POINT('Ctrl Pts',(13.8409250663671,8.40810721351364,2.77636606613607));
#13354=CARTESIAN_POINT('Ctrl Pts',(13.0339467396719,10.1105075714153,2.66522491860705));
#13355=CARTESIAN_POINT('Ctrl Pts',(14.0266158380486,11.7117536680222,2.55408377107803));
#13356=CARTESIAN_POINT('Ctrl Pts',(15.9102823145912,11.7461281313822,2.44294262354901));
#13357=CARTESIAN_POINT('Ctrl Pts',(16.9607123494012,10.182165940018,2.33180147601999));
#13358=CARTESIAN_POINT('Ctrl Pts',(16.2163838173521,8.45145624507036,2.22066032849097));
#13359=CARTESIAN_POINT('Ctrl Pts',(14.3586256307264,8.13822228853373,2.10951918096195));
#13360=CARTESIAN_POINT('Ctrl Pts',(13.0879561823328,9.52918602651344,1.99837803343293));
#13361=CARTESIAN_POINT('Ctrl Pts',(13.567496054586,11.3511142921827,1.88723688590391));
#13362=CARTESIAN_POINT('Ctrl Pts',(15.3582933952052,11.9362858933093,1.77609573837489));
#13363=CARTESIAN_POINT('Ctrl Pts',(16.8211231428988,10.7490580544729,1.66495459084587));
#13364=CARTESIAN_POINT('Ctrl Pts',(16.6169687348735,8.87617186592661,1.55381344331685));
#13365=CARTESIAN_POINT('Ctrl Pts',(14.9327051338352,8.0319939487841,1.44267229578783));
#13366=CARTESIAN_POINT('Ctrl Pts',(13.3100404788966,8.98925013270617,1.33153114825881));
#13367=CARTESIAN_POINT('Ctrl Pts',(13.2342981763212,10.8717083962423,1.22039000072979));
#13368=CARTESIAN_POINT('Ctrl Pts',(14.7748090869154,11.9562361327899,1.10924885320077));
#13369=CARTESIAN_POINT('Ctrl Pts',(16.5214516854989,11.2501087122817,0.99810770567175));
#13370=CARTESIAN_POINT('Ctrl Pts',(16.875415955447,9.39966945781174,0.886966558142732));
#13371=CARTESIAN_POINT('Ctrl Pts',(15.5127017221989,8.09877181111676,0.775825410613711));
#13372=CARTESIAN_POINT('Ctrl Pts',(13.6806745613723,8.53813915273012,0.664684263084692));
#13373=CARTESIAN_POINT('Ctrl Pts',(13.0563174575166,10.3157216649401,0.553543115555672));
#13374=CARTESIAN_POINT('Ctrl Pts',(14.2111078058336,11.8041392084987,0.442401968026652));
#13375=CARTESIAN_POINT('Ctrl Pts',(16.0880628853469,11.6414405555679,0.331260820497632));
#13376=CARTESIAN_POINT('Ctrl Pts',(16.9689629398242,9.97560865889059,0.220119672968611));
#13377=CARTESIAN_POINT('Ctrl Pts',(16.0477171708735,8.33331419534448,0.108978525439592));
#13378=CARTESIAN_POINT('Ctrl Pts',(14.167115703941,8.21427174764607,-0.00216262208942877));
#13379=CARTESIAN_POINT('Ctrl Pts',(13.0494874512438,9.73459567298507,-0.113303769618448));
#13380=CARTESIAN_POINT('Ctrl Pts',(13.4941166421103,10.9026562341787,-0.187397867971127));
#13381=CARTESIAN_POINT('Ctrl Pts',(13.9143317362933,11.2636773406136,-0.224444917147467));
#13382=CARTESIAN_POINT('Ctrl Pts',(16.3677806246588,11.1633123698097,8.07481497238249));
#13383=CARTESIAN_POINT('Ctrl Pts',(16.7546210002301,10.7084794424949,8.03776792320615));
#13384=CARTESIAN_POINT('Ctrl Pts',(17.032113047149,9.39033427232925,7.96367382485347));
#13385=CARTESIAN_POINT('Ctrl Pts',(15.5872663299559,7.95914173013072,7.85253267732445));
#13386=CARTESIAN_POINT('Ctrl Pts',(13.6050394565572,8.40125853894243,7.74139152979544));
#13387=CARTESIAN_POINT('Ctrl Pts',(12.8996447941346,10.3042276766854,7.6302503822664));
#13388=CARTESIAN_POINT('Ctrl Pts',(14.116859584488,11.9300353307635,7.5191092347374));
#13389=CARTESIAN_POINT('Ctrl Pts',(16.1424524326256,11.7884868836682,7.40796808720837));
#13390=CARTESIAN_POINT('Ctrl Pts',(17.1222965572413,10.010177926044,7.29682693967936));
#13391=CARTESIAN_POINT('Ctrl Pts',(16.1594706787569,8.22237212908425,7.18568579215033));
#13392=CARTESIAN_POINT('Ctrl Pts',(14.1353130595794,8.06182964697857,7.07454464462131));
#13393=CARTESIAN_POINT('Ctrl Pts',(12.9026547108187,9.67536368344986,6.9634034970923));
#13394=CARTESIAN_POINT('Ctrl Pts',(13.5898238192497,11.5860817277419,6.85226234956327));
#13395=CARTESIAN_POINT('Ctrl Pts',(15.5678121932987,12.0449504938755,6.74112120203425));
#13396=CARTESIAN_POINT('Ctrl Pts',(17.0260478674942,10.6319590149209,6.62998005450523));
#13397=CARTESIAN_POINT('Ctrl Pts',(16.6297193566359,8.64049384018613,6.51883890697621));
#13398=CARTESIAN_POINT('Ctrl Pts',(14.7416102143752,7.89346860809774,6.4076977594472));
#13399=CARTESIAN_POINT('Ctrl Pts',(13.0900208479722,9.07467802437696,6.29655661191817));
#13400=CARTESIAN_POINT('Ctrl Pts',(13.1867508941761,11.102891060296,6.18541546438915));
#13401=CARTESIAN_POINT('Ctrl Pts',(14.9432574787194,12.1215609826643,6.07427431686013));
#13402=CARTESIAN_POINT('Ctrl Pts',(16.7517039263869,11.1982379832749,5.96313316933111));
#13403=CARTESIAN_POINT('Ctrl Pts',(16.9567098535833,9.17809524326976,5.8519920218021));
#13404=CARTESIAN_POINT('Ctrl Pts',(15.3706209415879,7.91029165593742,5.74085087427306));
#13405=CARTESIAN_POINT('Ctrl Pts',(13.4452802721186,8.55532445140494,5.62970972674406));
#13406=CARTESIAN_POINT('Ctrl Pts',(12.9430685746236,10.5227561364266,5.51856857921503));
#13407=CARTESIAN_POINT('Ctrl Pts',(14.3236905813738,12.0116775172169,5.40742743168601));
#13408=CARTESIAN_POINT('Ctrl Pts',(16.3233794915402,11.6591888343887,5.296286284157));
#13409=CARTESIAN_POINT('Ctrl Pts',(17.1116991360081,9.78794428873115,5.18514513662797));
#13410=CARTESIAN_POINT('Ctrl Pts',(15.9670528791255,8.11080715799694,5.07400398909896));
#13411=CARTESIAN_POINT('Ctrl Pts',(13.937204649905,8.16296246373945,4.96286284156993));
#13412=CARTESIAN_POINT('Ctrl Pts',(12.8801972656884,9.89666930157111,4.85172169404092));
#13413=CARTESIAN_POINT('Ctrl Pts',(13.763573496338,11.7249609753961,4.74058054651189));
#13414=CARTESIAN_POINT('Ctrl Pts',(15.7787256653157,11.9742915701193,4.62943939898287));
#13415=CARTESIAN_POINT('Ctrl Pts',(17.0810631478139,10.4164337167515,4.51829825145386));
#13416=CARTESIAN_POINT('Ctrl Pts',(16.4784777013235,8.47738890312604,4.40715710392483));
#13417=CARTESIAN_POINT('Ctrl Pts',(14.5225522198569,7.93208208990784,4.29601595639582));
#13418=CARTESIAN_POINT('Ctrl Pts',(13.003663560048,9.27966557477885,4.18487480886679));
#13419=CARTESIAN_POINT('Ctrl Pts',(13.3121423505903,11.2866147134897,4.07373366133777));
#13420=CARTESIAN_POINT('Ctrl Pts',(15.1656193025807,12.1158476108296,3.96259251380876));
#13421=CARTESIAN_POINT('Ctrl Pts',(16.8674948928822,11.0083172569673,3.85145136627974));
#13422=CARTESIAN_POINT('Ctrl Pts',(16.8599394911652,8.97781315071892,3.74031021875072));
#13423=CARTESIAN_POINT('Ctrl Pts',(15.1498690134521,7.88297847331436,3.6291690712217));
#13424=CARTESIAN_POINT('Ctrl Pts',(13.3026143660185,8.72598160327735,3.51802792369268));
#13425=CARTESIAN_POINT('Ctrl Pts',(13.0090794204125,10.7351708042433,3.40688677616366));
#13426=CARTESIAN_POINT('Ctrl Pts',(14.5379544607021,12.0714137165907,3.29574562863464));
#13427=CARTESIAN_POINT('Ctrl Pts',(16.4897677203167,11.5115664077704,3.18460448110562));
#13428=CARTESIAN_POINT('Ctrl Pts',(17.0779065079348,9.56809097032502,3.0734633335766));
#13429=CARTESIAN_POINT('Ctrl Pts',(15.7640118298975,8.01996798268554,2.96232218604758));
#13430=CARTESIAN_POINT('Ctrl Pts',(13.750770928622,8.28428802168758,2.85118103851856));
#13431=CARTESIAN_POINT('Ctrl Pts',(12.8810249299575,10.1191029732536,2.74003989098954));
#13432=CARTESIAN_POINT('Ctrl Pts',(13.9509049350957,11.8448957725527,2.62889874346052));
#13433=CARTESIAN_POINT('Ctrl Pts',(15.9810850856591,11.8819439199126,2.5177575959315));
#13434=CARTESIAN_POINT('Ctrl Pts',(17.1132187371223,10.1963350094821,2.40661644840248));
#13435=CARTESIAN_POINT('Ctrl Pts',(16.3109955038258,8.33100878914221,2.29547530087346));
#13436=CARTESIAN_POINT('Ctrl Pts',(14.3087388187906,7.99341114701062,2.18433415334444));
#13437=CARTESIAN_POINT('Ctrl Pts',(12.9392352871511,9.49256559190101,2.07319300581542));
#13438=CARTESIAN_POINT('Ctrl Pts',(13.4560743041299,11.4562054648689,1.9620518582864));
#13439=CARTESIAN_POINT('Ctrl Pts',(15.3861618540659,12.0868923641024,1.85091071075738));
#13440=CARTESIAN_POINT('Ctrl Pts',(16.9627721268528,10.8073206232357,1.73976956322836));
#13441=CARTESIAN_POINT('Ctrl Pts',(16.7427383618607,8.78875926346142,1.62862841569934));
#13442=CARTESIAN_POINT('Ctrl Pts',(14.927470864283,7.87892024882208,1.51748726817032));
#13443=CARTESIAN_POINT('Ctrl Pts',(13.1785935473582,8.91063288362445,1.4063461206413));
#13444=CARTESIAN_POINT('Ctrl Pts',(13.0969599242293,10.9395108450296,1.29520497311228));
#13445=CARTESIAN_POINT('Ctrl Pts',(14.7572934871832,12.1083943554034,1.18406382558326));
#13446=CARTESIAN_POINT('Ctrl Pts',(16.6397918901283,11.3473435586001,1.07292267805424));
#13447=CARTESIAN_POINT('Ctrl Pts',(17.0212878947587,9.35297508040565,0.961781530525221));
#13448=CARTESIAN_POINT('Ctrl Pts',(15.552580232504,7.95089216757367,0.8506403829962));
#13449=CARTESIAN_POINT('Ctrl Pts',(13.5780559610789,8.42443398978971,0.739499235467181));
#13450=CARTESIAN_POINT('Ctrl Pts',(12.9051356671224,10.3402788472622,0.62835808793816));
#13451=CARTESIAN_POINT('Ctrl Pts',(14.1497468933721,11.9444671631413,0.517216940409142));
#13452=CARTESIAN_POINT('Ctrl Pts',(16.1726936269793,11.7691136279923,0.40607579288012));
#13453=CARTESIAN_POINT('Ctrl Pts',(17.1221110676466,9.97371147324507,0.2949346453511));
#13454=CARTESIAN_POINT('Ctrl Pts',(16.1292097779517,8.20367751936212,0.183793497822081));
#13455=CARTESIAN_POINT('Ctrl Pts',(14.1023330368556,8.07537581765355,0.0726523502930604));
#13456=CARTESIAN_POINT('Ctrl Pts',(12.8977744153637,9.71395222918213,-0.0384887972359591));
#13457=CARTESIAN_POINT('Ctrl Pts',(13.3769873593213,10.9728658402285,-0.112582895588638));
#13458=CARTESIAN_POINT('Ctrl Pts',(13.829887250996,11.361967569938,-0.149629944764978));
#13459=CARTESIAN_POINT('Ctrl Pts',(16.4664903694653,11.247266086571,8.14962994476498));
#13460=CARTESIAN_POINT('Ctrl Pts',(16.8812481713146,10.7596088587978,8.11258289558864));
#13461=CARTESIAN_POINT('Ctrl Pts',(17.1787662141011,9.34633602633083,8.03848879723595));
#13462=CARTESIAN_POINT('Ctrl Pts',(15.6296480602701,7.81185743952661,7.92734764970694));
#13463=CARTESIAN_POINT('Ctrl Pts',(13.5043681962864,8.28588085425572,7.81620650217792));
#13464=CARTESIAN_POINT('Ctrl Pts',(12.7480667394114,10.3261831246478,7.7050653546489));
#13465=CARTESIAN_POINT('Ctrl Pts',(14.0531252666655,12.0693217715365,7.59392420711989));
#13466=CARTESIAN_POINT('Ctrl Pts',(16.2249007332119,11.9175580817052,7.48278305959085));
#13467=CARTESIAN_POINT('Ctrl Pts',(17.2754580714433,10.0109124447704,7.37164191206185));
#13468=CARTESIAN_POINT('Ctrl Pts',(16.2431471490529,8.09408460231609,7.26050076453282));
#13469=CARTESIAN_POINT('Ctrl Pts',(14.0729104888107,7.92195611939011,7.1493596170038));
#13470=CARTESIAN_POINT('Ctrl Pts',(12.7512938752185,9.65193538845589,7.03821846947478));
#13471=CARTESIAN_POINT('Ctrl Pts',(13.488054479617,11.7005457870837,6.92707732194576));
#13472=CARTESIAN_POINT('Ctrl Pts',(15.6087899609963,12.1925301113618,6.81593617441674));
#13473=CARTESIAN_POINT('Ctrl Pts',(17.1722633236576,10.6775661188427,6.70479502688772));
#13474=CARTESIAN_POINT('Ctrl Pts',(16.7473326484895,8.54238124546246,6.5936538793587));
#13475=CARTESIAN_POINT('Ctrl Pts',(14.7229627870467,7.7414448314974,6.48251273182969));
#13476=CARTESIAN_POINT('Ctrl Pts',(12.9521818178798,9.00789955535137,6.37137158430065));
#13477=CARTESIAN_POINT('Ctrl Pts',(13.0558926605679,11.1824843029172,6.26023043677165));
#13478=CARTESIAN_POINT('Ctrl Pts',(14.9391624947034,12.2746694120531,6.14908928924261));
#13479=CARTESIAN_POINT('Ctrl Pts',(16.8781205786138,11.2847122053937,6.03794814171361));
#13480=CARTESIAN_POINT('Ctrl Pts',(17.0979213364961,9.11878016939794,5.92680699418458));
#13481=CARTESIAN_POINT('Ctrl Pts',(15.3973678466869,7.75948196201174,5.81566584665556));
#13482=CARTESIAN_POINT('Ctrl Pts',(13.333079539912,8.45106536763152,5.70452469912655));
#13483=CARTESIAN_POINT('Ctrl Pts',(12.794624319439,10.5604823067586,5.59338355159752));
#13484=CARTESIAN_POINT('Ctrl Pts',(14.2748828055367,12.1568558965399,5.4822424040685));
#13485=CARTESIAN_POINT('Ctrl Pts',(16.4188849034001,11.7789288741843,5.37110125653949));
#13486=CARTESIAN_POINT('Ctrl Pts',(17.2640958574308,9.77264069050295,5.25996010901046));
#13487=CARTESIAN_POINT('Ctrl Pts',(16.0368429764495,7.97446823056785,5.14881896148145));
#13488=CARTESIAN_POINT('Ctrl Pts',(13.8605050272477,8.03038747098476,5.03767781395242));
#13489=CARTESIAN_POINT('Ctrl Pts',(12.7272157252487,9.88921215041053,4.92653666642341));
#13490=CARTESIAN_POINT('Ctrl Pts',(13.6743432919849,11.8494476471713,4.81539551889438));
#13491=CARTESIAN_POINT('Ctrl Pts',(15.8349245983256,12.116771887172,4.70425437136536));
#13492=CARTESIAN_POINT('Ctrl Pts',(17.23124893678,10.446486829925,4.59311322383634));
#13493=CARTESIAN_POINT('Ctrl Pts',(16.5851762127431,8.36750538079628,4.48197207630733));
#13494=CARTESIAN_POINT('Ctrl Pts',(14.4880958547888,7.78284496408089,4.3708309287783));
#13495=CARTESIAN_POINT('Ctrl Pts',(12.8595923128151,9.22768061022607,4.25968978124929));
#13496=CARTESIAN_POINT('Ctrl Pts',(13.190333344936,11.3794668914948,4.14854863372026));
#13497=CARTESIAN_POINT('Ctrl Pts',(15.177571686463,12.268543718633,4.03740748619125));
#13498=CARTESIAN_POINT('Ctrl Pts',(17.0022679266424,11.0810853144502,3.92626633866222));
#13499=CARTESIAN_POINT('Ctrl Pts',(16.9941672680604,8.90404415500574,3.81512519113321));
#13500=CARTESIAN_POINT('Ctrl Pts',(15.1606847333165,7.73019764656371,3.70398404360418));
#13501=CARTESIAN_POINT('Ctrl Pts',(13.1801177464964,8.63403847398308,3.59284289607517));
#13502=CARTESIAN_POINT('Ctrl Pts',(12.8653990240112,10.7882264779147,3.48170174854614));
#13503=CARTESIAN_POINT('Ctrl Pts',(14.5046096417664,12.220903127149,3.37056060101713));
#13504=CARTESIAN_POINT('Ctrl Pts',(16.5972810077856,11.620652858974,3.2594194534881));
#13505=CARTESIAN_POINT('Ctrl Pts',(17.2278644890848,9.53692103756665,3.14827830595909));
#13506=CARTESIAN_POINT('Ctrl Pts',(15.8191488974935,7.87707339007757,3.03713715843007));
#13507=CARTESIAN_POINT('Ctrl Pts',(13.660616790877,8.16046882986155,2.92599601090105));
#13508=CARTESIAN_POINT('Ctrl Pts',(12.7281031202431,10.1276983750918,2.81485486337203));
#13509=CARTESIAN_POINT('Ctrl Pts',(13.8751940321428,11.9780378770833,2.703713715843));
#13510=CARTESIAN_POINT('Ctrl Pts',(16.051887856727,12.017759708443,2.59257256831399));
#13511=CARTESIAN_POINT('Ctrl Pts',(17.2657251248433,10.2105040789463,2.48143142078496));
#13512=CARTESIAN_POINT('Ctrl Pts',(16.4056071902996,8.21056133321405,2.37029027325595));
#13513=CARTESIAN_POINT('Ctrl Pts',(14.2588520068548,7.84860000548751,2.25914912572693));
#13514=CARTESIAN_POINT('Ctrl Pts',(12.7905143919695,9.45594515728858,2.14800797819791));
#13515=CARTESIAN_POINT('Ctrl Pts',(13.3446525536738,11.5612966375552,2.03686683066889));
#13516=CARTESIAN_POINT('Ctrl Pts',(15.4140303129267,12.2374988348955,1.92572568313987));
#13517=CARTESIAN_POINT('Ctrl Pts',(17.1044211108068,10.8655831919985,1.81458453561085));
#13518=CARTESIAN_POINT('Ctrl Pts',(16.868507988848,8.70134666099622,1.70344338808183));
#13519=CARTESIAN_POINT('Ctrl Pts',(14.9222365947309,7.72584654886007,1.59230224055281));
#13520=CARTESIAN_POINT('Ctrl Pts',(13.0471466158198,8.83201563454272,1.48116109302379));
#13521=CARTESIAN_POINT('Ctrl Pts',(12.9596216721374,11.007313293817,1.37001994549477));
#13522=CARTESIAN_POINT('Ctrl Pts',(14.7397778874509,12.2605525780168,1.25887879796575));
#13523=CARTESIAN_POINT('Ctrl Pts',(16.7581320947577,11.4445784049186,1.14773765043673));
#13524=CARTESIAN_POINT('Ctrl Pts',(17.1671598340705,9.30628070299953,1.03659650290771));
#13525=CARTESIAN_POINT('Ctrl Pts',(15.5924587428091,7.80301252403059,0.925455355378689));
#13526=CARTESIAN_POINT('Ctrl Pts',(13.4754373607854,8.3107288268493,0.81431420784967));
#13527=CARTESIAN_POINT('Ctrl Pts',(12.7539538767281,10.3648360295842,0.703173060320649));
#13528=CARTESIAN_POINT('Ctrl Pts',(14.0883859809107,12.084795117784,0.592031912791631));
#13529=CARTESIAN_POINT('Ctrl Pts',(16.2573243686117,11.8967867004167,0.480890765262609));
#13530=CARTESIAN_POINT('Ctrl Pts',(17.2752591954691,9.97181428759956,0.36974961773359));
#13531=CARTESIAN_POINT('Ctrl Pts',(16.21070238503,8.07404084337976,0.25860847020457));
#13532=CARTESIAN_POINT('Ctrl Pts',(14.0375503697701,7.93647988766104,0.147467322675549));
#13533=CARTESIAN_POINT('Ctrl Pts',(12.7460613794835,9.6933087853792,0.03632617514653));
#13534=CARTESIAN_POINT('Ctrl Pts',(13.2598580765322,11.0430754462783,-0.0377679232061492));
#13535=CARTESIAN_POINT('Ctrl Pts',(13.7454427656987,11.4602577992624,-0.0748149723824891));
#13536=CARTESIAN_POINT('Ctrl Pts',(16.5652001142717,11.3312198033322,8.22444491714747));
#13537=CARTESIAN_POINT('Ctrl Pts',(17.0078753423991,10.8107382751008,8.18739786797113));
#13538=CARTESIAN_POINT('Ctrl Pts',(17.3254193810532,9.3023377803324,8.11330376961845));
#13539=CARTESIAN_POINT('Ctrl Pts',(15.6720297905844,7.66457314892251,8.00216262208943));
#13540=CARTESIAN_POINT('Ctrl Pts',(13.4036969360157,8.170503169569,7.89102147456041));
#13541=CARTESIAN_POINT('Ctrl Pts',(12.5964886846882,10.3481385726101,7.77988032703139));
#13542=CARTESIAN_POINT('Ctrl Pts',(13.989390948843,12.2086082123096,7.66873917950236));
#13543=CARTESIAN_POINT('Ctrl Pts',(16.3073490337982,12.0466292797422,7.55759803197335));
#13544=CARTESIAN_POINT('Ctrl Pts',(17.4286195856453,10.0116469634969,7.44645688444433));
#13545=CARTESIAN_POINT('Ctrl Pts',(16.3268236193488,7.9657970755479,7.33531573691531));
#13546=CARTESIAN_POINT('Ctrl Pts',(14.0105079180419,7.78208259180166,7.22417458938629));
#13547=CARTESIAN_POINT('Ctrl Pts',(12.5999330396184,9.6285070934619,7.11303344185727));
#13548=CARTESIAN_POINT('Ctrl Pts',(13.3862851399842,11.8150098464255,7.00189229432825));
#13549=CARTESIAN_POINT('Ctrl Pts',(15.6497677286939,12.3401097288481,6.89075114679923));
#13550=CARTESIAN_POINT('Ctrl Pts',(17.3184787798211,10.7231732227644,6.77960999927021));
#13551=CARTESIAN_POINT('Ctrl Pts',(16.864945940343,8.44426865073882,6.66846885174118));
#13552=CARTESIAN_POINT('Ctrl Pts',(14.7043153597183,7.58942105489702,6.55732770421218));
#13553=CARTESIAN_POINT('Ctrl Pts',(12.8143427877872,8.94112108632582,6.44618655668314));
#13554=CARTESIAN_POINT('Ctrl Pts',(12.9250344269597,11.2620775455385,6.33504540915413));
#13555=CARTESIAN_POINT('Ctrl Pts',(14.9350675106875,12.4277778414421,6.22390426162511));
#13556=CARTESIAN_POINT('Ctrl Pts',(17.0045372308406,11.3711864275124,6.1127631140961));
#13557=CARTESIAN_POINT('Ctrl Pts',(17.2391328194089,9.05946509552617,6.00162196656707));
#13558=CARTESIAN_POINT('Ctrl Pts',(15.424114751786,7.608672268086,5.89048081903805));
#13559=CARTESIAN_POINT('Ctrl Pts',(13.2208788077054,8.34680628385815,5.77933967150903));
#13560=CARTESIAN_POINT('Ctrl Pts',(12.6461800642546,10.5982084770906,5.66819852398001));
#13561=CARTESIAN_POINT('Ctrl Pts',(14.2260750296995,12.3020342758629,5.55705737645099));
#13562=CARTESIAN_POINT('Ctrl Pts',(16.51439031526,11.8986689139798,5.44591622892198));
#13563=CARTESIAN_POINT('Ctrl Pts',(17.4164925788533,9.75733709227475,5.33477508139295));
#13564=CARTESIAN_POINT('Ctrl Pts',(16.1066330737735,7.83812930313874,5.22363393386394));
#13565=CARTESIAN_POINT('Ctrl Pts',(13.7838054045903,7.89781247823008,5.11249278633491));
#13566=CARTESIAN_POINT('Ctrl Pts',(12.574234184809,9.88175499924995,5.0013516388059));
#13567=CARTESIAN_POINT('Ctrl Pts',(13.5851130876319,11.9739343189466,4.89021049127687));
#13568=CARTESIAN_POINT('Ctrl Pts',(15.8911235313356,12.2592522042247,4.77906934374785));
#13569=CARTESIAN_POINT('Ctrl Pts',(17.381434725746,10.4765399430985,4.66792819621883));
#13570=CARTESIAN_POINT('Ctrl Pts',(16.6918747241627,8.25762185846654,4.55678704868982));
#13571=CARTESIAN_POINT('Ctrl Pts',(14.4536394897207,7.63360783825394,4.44564590116079));
#13572=CARTESIAN_POINT('Ctrl Pts',(12.7155210655824,9.17569564567328,4.33450475363177));
#13573=CARTESIAN_POINT('Ctrl Pts',(13.0685243392818,11.4723190694999,4.22336360610275));
#13574=CARTESIAN_POINT('Ctrl Pts',(15.1895240703454,12.4212398264365,4.11222245857373));
#13575=CARTESIAN_POINT('Ctrl Pts',(17.1370409604027,11.1538533719331,4.00108131104472));
#13576=CARTESIAN_POINT('Ctrl Pts',(17.1283950449557,8.83027515929254,3.88994016351569));
#13577=CARTESIAN_POINT('Ctrl Pts',(15.1715004531809,7.57741681981306,3.77879901598667));
#13578=CARTESIAN_POINT('Ctrl Pts',(13.0576211269744,8.54209534468881,3.66765786845765));
#13579=CARTESIAN_POINT('Ctrl Pts',(12.7217186276099,10.8412821515861,3.55651672092863));
#13580=CARTESIAN_POINT('Ctrl Pts',(14.4712648228307,12.3703925377072,3.44537557339962));
#13581=CARTESIAN_POINT('Ctrl Pts',(16.7047942952545,11.7297393101775,3.33423442587059));
#13582=CARTESIAN_POINT('Ctrl Pts',(17.3778224702348,9.50575110480829,3.22309327834158));
#13583=CARTESIAN_POINT('Ctrl Pts',(15.8742859650895,7.73417879746959,3.11195213081255));
#13584=CARTESIAN_POINT('Ctrl Pts',(13.5704626531319,8.0366496380355,3.00081098328354));
#13585=CARTESIAN_POINT('Ctrl Pts',(12.5751813105287,10.1362937769301,2.88966983575452));
#13586=CARTESIAN_POINT('Ctrl Pts',(13.79948312919,12.1111799816138,2.77852868822549));
#13587=CARTESIAN_POINT('Ctrl Pts',(16.1226906277949,12.1535754969733,2.66738754069648));
#13588=CARTESIAN_POINT('Ctrl Pts',(17.4182315125643,10.2246731484105,2.55624639316745));
#13589=CARTESIAN_POINT('Ctrl Pts',(16.5002188767733,8.09011387728591,2.44510524563844));
#13590=CARTESIAN_POINT('Ctrl Pts',(14.208965194919,7.70378886396441,2.33396409810942));
#13591=CARTESIAN_POINT('Ctrl Pts',(12.6417934967878,9.41932472267615,2.2228229505804));
#13592=CARTESIAN_POINT('Ctrl Pts',(13.2332308032177,11.6663878102415,2.11168180305138));
#13593=CARTESIAN_POINT('Ctrl Pts',(15.4418987717874,12.3881053056886,2.00054065552236));
#13594=CARTESIAN_POINT('Ctrl Pts',(17.2460700947607,10.9238457607613,1.88939950799334));
#13595=CARTESIAN_POINT('Ctrl Pts',(16.9942776158352,8.61393405853105,1.77825836046432));
#13596=CARTESIAN_POINT('Ctrl Pts',(14.9170023251788,7.57277284889803,1.6671172129353));
#13597=CARTESIAN_POINT('Ctrl Pts',(12.9156996842814,8.75339838546101,1.55597606540628));
#13598=CARTESIAN_POINT('Ctrl Pts',(12.8222834200456,11.0751157426043,1.44483491787726));
#13599=CARTESIAN_POINT('Ctrl Pts',(14.7222622877187,12.4127108006303,1.33369377034824));
#13600=CARTESIAN_POINT('Ctrl Pts',(16.8764722993871,11.541813251237,1.22255262281922));
#13601=CARTESIAN_POINT('Ctrl Pts',(17.3130317733822,9.25958632559344,1.1114114752902));
#13602=CARTESIAN_POINT('Ctrl Pts',(15.6323372531142,7.65513288048749,1.00027032776118));
#13603=CARTESIAN_POINT('Ctrl Pts',(13.372818760492,8.19702366390889,0.889129180232159));
#13604=CARTESIAN_POINT('Ctrl Pts',(12.6027720863339,10.3893932119062,0.777988032703138));
#13605=CARTESIAN_POINT('Ctrl Pts',(14.0270250684493,12.2251230724266,0.66684688517412));
#13606=CARTESIAN_POINT('Ctrl Pts',(16.3419551102441,12.024459772841,0.555705737645098));
#13607=CARTESIAN_POINT('Ctrl Pts',(17.4284073232916,9.96991710195404,0.444564590116078));
#13608=CARTESIAN_POINT('Ctrl Pts',(16.2921949921082,7.9444041673974,0.333423442587059));
#13609=CARTESIAN_POINT('Ctrl Pts',(13.9727677026847,7.79758395766853,0.222282295058038));
#13610=CARTESIAN_POINT('Ctrl Pts',(12.5943483436034,9.67266534157626,0.111141147529019));
#13611=CARTESIAN_POINT('Ctrl Pts',(13.1427287937432,11.1132850523281,0.0370470491763399));
#13612=CARTESIAN_POINT('Ctrl Pts',(13.6609982804014,11.5585480285869,0.));
#13613=CARTESIAN_POINT('Ctrl Pts',(16.2690708798524,11.0793586530485,8.));
#13614=CARTESIAN_POINT('Ctrl Pts',(16.314784652283,11.0367125551188,8.));
#13615=CARTESIAN_POINT('Ctrl Pts',(16.357765226135,10.9914157787626,8.));
#13616=CARTESIAN_POINT('Ctrl Pts',(16.3980010208502,10.943805412763,8.));
#13617=CARTESIAN_POINT('Ctrl Pts',(16.4235329118048,10.9135939385864,8.));
#13618=CARTESIAN_POINT('Ctrl Pts',(16.4479591518653,10.8824498539581,8.));
#13619=CARTESIAN_POINT('Ctrl Pts',(16.4712714314018,10.8504502532411,8.));
#13620=CARTESIAN_POINT('Ctrl Pts',(16.4873491735028,10.8283811404005,8.));
#13621=CARTESIAN_POINT('Ctrl Pts',(16.5028969805187,10.8059049651785,8.));
#13622=CARTESIAN_POINT('Ctrl Pts',(16.5179108032207,10.7830453876846,8.));
#13623=CARTESIAN_POINT('Ctrl Pts',(16.5257295949839,10.7711407395634,8.));
#13624=CARTESIAN_POINT('Ctrl Pts',(16.5334031154624,10.759132546163,8.));
#13625=CARTESIAN_POINT('Ctrl Pts',(16.5409237973063,10.7470358005141,8.));
#13626=CARTESIAN_POINT('Ctrl Pts',(16.5757596995797,10.6910035074322,8.));
#13627=CARTESIAN_POINT('Ctrl Pts',(16.607360581433,10.6330123468312,8.));
#13628=CARTESIAN_POINT('Ctrl Pts',(16.6356935185973,10.5734135013109,8.));
#13629=CARTESIAN_POINT('Ctrl Pts',(16.65611782791,10.5304505974462,8.));
#13630=CARTESIAN_POINT('Ctrl Pts',(16.6748433410819,10.4866511989788,8.));
#13631=CARTESIAN_POINT('Ctrl Pts',(16.6918460893235,10.4421348904576,8.));
#13632=CARTESIAN_POINT('Ctrl Pts',(16.6965919783289,10.4297092839518,8.));
#13633=CARTESIAN_POINT('Ctrl Pts',(16.7012035820491,10.4172277727484,8.));
#13634=CARTESIAN_POINT('Ctrl Pts',(16.7056802275322,10.4046928500131,8.));
#13635=CARTESIAN_POINT('Ctrl Pts',(16.710058403887,10.3924336477742,8.));
#13636=CARTESIAN_POINT('Ctrl Pts',(16.7143044894992,10.380131701097,8.));
#13637=CARTESIAN_POINT('Ctrl Pts',(16.7184173516006,10.367792630208,8.));
#13638=CARTESIAN_POINT('Ctrl Pts',(16.7398742805331,10.3034193153175,8.));
#13639=CARTESIAN_POINT('Ctrl Pts',(16.7577174338981,10.2380126755093,8.));
#13640=CARTESIAN_POINT('Ctrl Pts',(16.7719142685079,10.1719289098357,8.));
#13641=CARTESIAN_POINT('Ctrl Pts',(16.7863147862362,10.1048970351052,8.));
#13642=CARTESIAN_POINT('Ctrl Pts',(16.796964156607,10.0371675551568,8.));
#13643=CARTESIAN_POINT('Ctrl Pts',(16.8037861146634,9.96908054818257,8.));
#13644=CARTESIAN_POINT('Ctrl Pts',(16.8080115895847,9.92690791415968,8.));
#13645=CARTESIAN_POINT('Ctrl Pts',(16.8107678210036,9.88459754218389,8.));
#13646=CARTESIAN_POINT('Ctrl Pts',(16.8120273023581,9.8422266950913,8.));
#13647=CARTESIAN_POINT('Ctrl Pts',(16.813060369613,9.80747275885079,8.));
#13648=CARTESIAN_POINT('Ctrl Pts',(16.8130863293521,9.77267806685123,8.));
#13649=CARTESIAN_POINT('Ctrl Pts',(16.8120860218337,9.73788470224784,8.));
#13650=CARTESIAN_POINT('Ctrl Pts',(16.8116793102994,9.7237381898587,8.));
#13651=CARTESIAN_POINT('Ctrl Pts',(16.8111026395985,9.70958947886931,8.));
#13652=CARTESIAN_POINT('Ctrl Pts',(16.810356201727,9.69546521518563,8.));
#13653=CARTESIAN_POINT('Ctrl Pts',(16.8066366250451,9.62508255663006,8.));
#13654=CARTESIAN_POINT('Ctrl Pts',(16.7987033737293,9.55518330023832,8.));
#13655=CARTESIAN_POINT('Ctrl Pts',(16.7864936208905,9.48612488219693,8.));
#13656=CARTESIAN_POINT('Ctrl Pts',(16.7851385866999,9.47846080260131,8.));
#13657=CARTESIAN_POINT('Ctrl Pts',(16.7837308318786,9.47080705979357,8.));
#13658=CARTESIAN_POINT('Ctrl Pts',(16.782270233023,9.46316412952721,8.));
#13659=CARTESIAN_POINT('Ctrl Pts',(16.7696151815605,9.39694356837038,8.));
#13660=CARTESIAN_POINT('Ctrl Pts',(16.7529975308864,9.33153486627218,8.));
#13661=CARTESIAN_POINT('Ctrl Pts',(16.7326883279903,9.26714561729205,8.));
#13662=CARTESIAN_POINT('Ctrl Pts',(16.7108362800783,9.19786486014313,8.));
#13663=CARTESIAN_POINT('Ctrl Pts',(16.6847107136327,9.12976334731771,8.));
#13664=CARTESIAN_POINT('Ctrl Pts',(16.6545852471777,9.06310545296145,8.));
#13665=CARTESIAN_POINT('Ctrl Pts',(16.6490327135744,9.05081949553446,8.));
#13666=CARTESIAN_POINT('Ctrl Pts',(16.6433441297437,9.03858262010034,8.));
#13667=CARTESIAN_POINT('Ctrl Pts',(16.6375209875576,9.02639654643794,8.));
#13668=CARTESIAN_POINT('Ctrl Pts',(16.6325866305862,9.01607043115377,8.));
#13669=CARTESIAN_POINT('Ctrl Pts',(16.6275597790168,9.0057894375504,8.));
#13670=CARTESIAN_POINT('Ctrl Pts',(16.6224422427912,8.99555531601222,8.));
#13671=CARTESIAN_POINT('Ctrl Pts',(16.5906563609555,8.93198945862292,8.));
#13672=CARTESIAN_POINT('Ctrl Pts',(16.5553715219545,8.87022144200131,8.));
#13673=CARTESIAN_POINT('Ctrl Pts',(16.5168958154538,8.81047563769863,8.));
#13674=CARTESIAN_POINT('Ctrl Pts',(16.4776074025218,8.74946784748795,8.));
#13675=CARTESIAN_POINT('Ctrl Pts',(16.4349915420324,8.69056773410278,8.));
#13676=CARTESIAN_POINT('Ctrl Pts',(16.3893217542466,8.63402247023065,8.));
#13677=CARTESIAN_POINT('Ctrl Pts',(16.3433740602154,8.5771331215108,8.));
#13678=CARTESIAN_POINT('Ctrl Pts',(16.2943346227761,8.522626437839,8.));
#13679=CARTESIAN_POINT('Ctrl Pts',(16.2424343742239,8.47077604070952,8.));
#13680=CARTESIAN_POINT('Ctrl Pts',(16.2296036049381,8.45795759568269,8.));
#13681=CARTESIAN_POINT('Ctrl Pts',(16.2165977853048,8.44530163917201,8.));
#13682=CARTESIAN_POINT('Ctrl Pts',(16.2034200194896,8.43281261409566,8.));
#13683=CARTESIAN_POINT('Ctrl Pts',(16.1931256240804,8.42305625901894,8.));
#13684=CARTESIAN_POINT('Ctrl Pts',(16.1827250344693,8.41340078989772,8.));
#13685=CARTESIAN_POINT('Ctrl Pts',(16.172235821794,8.40386260566874,8.));
#13686=CARTESIAN_POINT('Ctrl Pts',(16.1164871858091,8.35316854721106,8.));
#13687=CARTESIAN_POINT('Ctrl Pts',(16.0581411327798,8.30569128093942,8.));
#13688=CARTESIAN_POINT('Ctrl Pts',(15.9974954185764,8.26168435413653,8.));
#13689=CARTESIAN_POINT('Ctrl Pts',(15.9367829241817,8.2176289689879,8.));
#13690=CARTESIAN_POINT('Ctrl Pts',(15.873765062306,8.17705063925328,8.));
#13691=CARTESIAN_POINT('Ctrl Pts',(15.8086958538675,8.14023020006429,8.));
#13692=CARTESIAN_POINT('Ctrl Pts',(15.745109232976,8.10424870645226,8.));
#13693=CARTESIAN_POINT('Ctrl Pts',(15.6795629473788,8.07185507016062,8.));
#13694=CARTESIAN_POINT('Ctrl Pts',(15.6122617289213,8.0433487143013,8.));
#13695=CARTESIAN_POINT('Ctrl Pts',(15.597755809183,8.03720453267124,8.));
#13696=CARTESIAN_POINT('Ctrl Pts',(15.5831682628234,8.03124110383924,8.));
#13697=CARTESIAN_POINT('Ctrl Pts',(15.5685009870302,8.0254617116896,8.));
#13698=CARTESIAN_POINT('Ctrl Pts',(15.5561467177936,8.02059372068384,8.));
#13699=CARTESIAN_POINT('Ctrl Pts',(15.5437358816804,8.01585630076653,8.));
#13700=CARTESIAN_POINT('Ctrl Pts',(15.531270276981,8.01124903105919,8.));
#13701=CARTESIAN_POINT('Ctrl Pts',(13.3326898978632,9.99870038716915,6.87148036339021));
#13702=CARTESIAN_POINT('Ctrl Pts',(13.331960273942,9.91361837560012,6.87718308383007));
#13703=CARTESIAN_POINT('Ctrl Pts',(13.3379104352826,9.82863878514235,6.88288580426994));
#13704=CARTESIAN_POINT('Ctrl Pts',(13.3508951624844,9.74474812612374,6.8885885247098));
#13705=CARTESIAN_POINT('Ctrl Pts',(13.4352489077286,9.19976237715157,6.92563557388614));
#13706=CARTESIAN_POINT('Ctrl Pts',(13.8164822690384,8.7007327758593,6.96268262306248));
#13707=CARTESIAN_POINT('Ctrl Pts',(14.3201120460454,8.4760440554274,6.99972967223882));
#13708=CARTESIAN_POINT('Ctrl Pts',(14.8237418230524,8.2513553349955,7.03677672141516));
#13709=CARTESIAN_POINT('Ctrl Pts',(15.4497680157567,8.30100749542397,7.0738237705915));
#13710=CARTESIAN_POINT('Ctrl Pts',(15.9116712512052,8.60229753421573,7.11087081976784));
#13711=CARTESIAN_POINT('Ctrl Pts',(16.3735744866537,8.90358757300749,7.14791786894418));
#13712=CARTESIAN_POINT('Ctrl Pts',(16.6713547648465,9.45651549016254,7.18496491812052));
#13713=CARTESIAN_POINT('Ctrl Pts',(16.6687230854429,10.007974828459,7.22201196729686));
#13714=CARTESIAN_POINT('Ctrl Pts',(16.6660914060393,10.5594341667554,7.2590590164732));
#13715=CARTESIAN_POINT('Ctrl Pts',(16.3630477690393,11.1094249261933,7.29610606564954));
#13716=CARTESIAN_POINT('Ctrl Pts',(15.8982909122512,11.4063091733054,7.33315311482588));
#13717=CARTESIAN_POINT('Ctrl Pts',(15.433534055463,11.7031934204176,7.37020016400222));
#13718=CARTESIAN_POINT('Ctrl Pts',(14.8070639788868,11.746971155204,7.40724721317856));
#13719=CARTESIAN_POINT('Ctrl Pts',(14.3056004316898,11.5174472457193,7.4442942623549));
#13720=CARTESIAN_POINT('Ctrl Pts',(13.8041368844929,11.2879233362346,7.48134131153124));
#13721=CARTESIAN_POINT('Ctrl Pts',(13.4276798666754,10.7850977824788,7.51838836070758));
#13722=CARTESIAN_POINT('Ctrl Pts',(13.3485326690949,10.2394123380852,7.55543540988392));
#13723=CARTESIAN_POINT('Ctrl Pts',(13.3371065399469,10.1606341557557,7.56078372771935));
#13724=CARTESIAN_POINT('Ctrl Pts',(13.3318767677375,10.0809627127174,7.56613204555478));
#13725=CARTESIAN_POINT('Ctrl Pts',(13.3325428889984,10.0012066618994,7.57148036339021));
#13726=CARTESIAN_POINT('Ctrl Pts',(14.4698297828114,8.01482567432828,8.));
#13727=CARTESIAN_POINT('Ctrl Pts',(13.8096927451188,8.1911250512252,7.96295295082366));
#13728=CARTESIAN_POINT('Ctrl Pts',(12.6905567406518,9.25114015972233,7.88885885247099));
#13729=CARTESIAN_POINT('Ctrl Pts',(13.1189039003815,11.5386115720214,7.77771770494195));
#13730=CARTESIAN_POINT('Ctrl Pts',(15.2723377259255,12.4126882042673,7.66657655741295));
#13731=CARTESIAN_POINT('Ctrl Pts',(17.1748665662283,11.0807510628696,7.55543540988391));
#13732=CARTESIAN_POINT('Ctrl Pts',(17.0874397300721,8.75827685188236,7.44429426235491));
#13733=CARTESIAN_POINT('Ctrl Pts',(15.0888245216199,7.57307606901691,7.33315311482588));
#13734=CARTESIAN_POINT('Ctrl Pts',(13.0091239883167,8.60905062621059,7.22201196729686));
#13735=CARTESIAN_POINT('Ctrl Pts',(12.7516785328344,10.9184180508126,7.11087081976784));
#13736=CARTESIAN_POINT('Ctrl Pts',(14.552316547407,12.3870127270114,6.99972967223883));
#13737=CARTESIAN_POINT('Ctrl Pts',(16.7627159052523,11.6706763447836,6.8885885247098));
#13738=CARTESIAN_POINT('Ctrl Pts',(17.359610496679,9.42504513942049,6.77744737718079));
#13739=CARTESIAN_POINT('Ctrl Pts',(15.796602835303,7.70571713781293,6.66630622965176));
#13740=CARTESIAN_POINT('Ctrl Pts',(13.5044206094209,8.08647863727104,6.55516508212274));
#13741=CARTESIAN_POINT('Ctrl Pts',(12.581230473367,10.218805203436,6.44402393459371));
#13742=CARTESIAN_POINT('Ctrl Pts',(13.8720874462699,12.1508444526632,6.33288278706471));
#13743=CARTESIAN_POINT('Ctrl Pts',(16.1953904039119,12.1140865945272,6.22174163953568));
#13744=CARTESIAN_POINT('Ctrl Pts',(17.4244805427636,10.1421770013196,6.11060049200667));
#13745=CARTESIAN_POINT('Ctrl Pts',(16.4342968937075,8.04012443367538,5.99945934447764));
#13746=CARTESIAN_POINT('Ctrl Pts',(14.1312146531314,7.73206435471271,5.88831819694863));
#13747=CARTESIAN_POINT('Ctrl Pts',(12.6233841302342,9.49998296241927,5.77717704941961));
#13748=CARTESIAN_POINT('Ctrl Pts',(13.2910138340933,11.7255973659335,5.66603590189058));
#13749=CARTESIAN_POINT('Ctrl Pts',(15.5229818972268,12.3716681799822,5.55489475436157));
#13750=CARTESIAN_POINT('Ctrl Pts',(17.2762330137476,10.8468076994282,5.44375360683255));
#13751=CARTESIAN_POINT('Ctrl Pts',(16.9459104193154,8.54681293441946,5.33261245930352));
#13752=CARTESIAN_POINT('Ctrl Pts',(14.8343783616792,7.57700815405708,5.22147131177451));
#13753=CARTESIAN_POINT('Ctrl Pts',(12.874449803007,8.82511431568684,5.11033016424549));
#13754=CARTESIAN_POINT('Ctrl Pts',(12.8601658597075,11.1486643820772,4.99918901671646));
#13755=CARTESIAN_POINT('Ctrl Pts',(14.8046014881481,12.4207724868025,4.88804786918745));
#13756=CARTESIAN_POINT('Ctrl Pts',(16.9278971892049,11.4770011641531,4.77690672165842));
#13757=CARTESIAN_POINT('Ctrl Pts',(17.2864720241886,9.18124137035986,4.66576557412941));
#13758=CARTESIAN_POINT('Ctrl Pts',(15.5521007657847,7.63494085580992,4.55462442660038));
#13759=CARTESIAN_POINT('Ctrl Pts',(13.3123582941187,8.25352197734149,4.44348327907137));
#13760=CARTESIAN_POINT('Ctrl Pts',(12.6174163177399,10.4707600323777,4.33234213154234));
#13761=CARTESIAN_POINT('Ctrl Pts',(14.1033972467191,12.2570829656611,4.22120098401333));
#13762=CARTESIAN_POINT('Ctrl Pts',(16.4100928881365,11.9773613877815,4.11005983648431));
#13763=CARTESIAN_POINT('Ctrl Pts',(17.4260452489189,9.88764137211515,3.99891868895528));
#13764=CARTESIAN_POINT('Ctrl Pts',(16.2212917045089,7.90077000222407,3.88777754142627));
#13765=CARTESIAN_POINT('Ctrl Pts',(13.8986160185493,7.83545077753679,3.77663639389725));
#13766=CARTESIAN_POINT('Ctrl Pts',(12.584103685101,9.7514743338816,3.66549524636823));
#13767=CARTESIAN_POINT('Ctrl Pts',(13.4810073238894,11.8949884593291,3.5543540988392));
#13768=CARTESIAN_POINT('Ctrl Pts',(15.7683368037833,12.3039050690097,3.44321295131019));
#13769=CARTESIAN_POINT('Ctrl Pts',(17.3523611503097,10.6039180652812,3.33207180378117));
#13770=CARTESIAN_POINT('Ctrl Pts',(16.7831271023553,8.35112834097283,3.22093065625215));
#13771=CARTESIAN_POINT('Ctrl Pts',(14.5816890022697,7.60765054388266,3.10978950872313));
#13772=CARTESIAN_POINT('Ctrl Pts',(12.7631562512648,9.05403485540002,2.99864836119411));
#13773=CARTESIAN_POINT('Ctrl Pts',(12.9921418323749,11.366318260873,2.88750721366509));
#13774=CARTESIAN_POINT('Ctrl Pts',(15.0590413979142,12.4279279486728,2.77636606613607));
#13775=CARTESIAN_POINT('Ctrl Pts',(17.071896801884,11.2671083826901,2.66522491860705));
#13776=CARTESIAN_POINT('Ctrl Pts',(17.1882197878565,8.94642789870889,2.55408377107803));
#13777=CARTESIAN_POINT('Ctrl Pts',(15.3015328924376,7.59014566366572,2.44294262354901));
#13778=CARTESIAN_POINT('Ctrl Pts',(13.138834709854,8.43974881014599,2.33180147601999));
#13779=CARTESIAN_POINT('Ctrl Pts',(12.6797736488162,10.7175442146931,2.22066032849097));
#13780=CARTESIAN_POINT('Ctrl Pts',(14.3445560622211,12.3385280047513,2.10951918096195));
#13781=CARTESIAN_POINT('Ctrl Pts',(16.6093059338468,11.8189157324019,1.99837803343293));
#13782=CARTESIAN_POINT('Ctrl Pts',(17.4009607961183,9.63433987693309,1.88723688590391));
#13783=CARTESIAN_POINT('Ctrl Pts',(15.9948710360845,7.78447490731078,1.77609573837489));
#13784=CARTESIAN_POINT('Ctrl Pts',(13.6781157275128,7.96261388733151,1.66495459084587));
#13785=CARTESIAN_POINT('Ctrl Pts',(12.5713608945246,10.0056958124789,1.55381344331685));
#13786=CARTESIAN_POINT('Ctrl Pts',(13.6876865240177,12.0435635368564,1.44267229578783));
#13787=CARTESIAN_POINT('Ctrl Pts',(16.0052515541106,12.2108349221453,1.33153114825881));
#13788=CARTESIAN_POINT('Ctrl Pts',(17.402649969509,10.3543936274306,1.22039000072979));
#13789=CARTESIAN_POINT('Ctrl Pts',(16.6007558214423,8.1735579042694,1.10924885320077));
#13790=CARTESIAN_POINT('Ctrl Pts',(14.333596515509,7.6645683089416,0.998107705671753));
#13791=CARTESIAN_POINT('Ctrl Pts',(12.6764299583764,9.29335364338448,0.886966558142731));
#13792=CARTESIAN_POINT('Ctrl Pts',(13.1461804472137,11.5689497437289,0.775825410613713));
#13793=CARTESIAN_POINT('Ctrl Pts',(15.3128190766481,12.4084404416678,0.664684263084692));
#13794=CARTESIAN_POINT('Ctrl Pts',(17.1931639076296,11.0432447117585,0.553543115555672));
#13795=CARTESIAN_POINT('Ctrl Pts',(17.0658793839574,8.72328862566383,0.442401968026654));
#13796=CARTESIAN_POINT('Ctrl Pts',(15.0477523711852,7.57162591137588,0.331260820497632));
#13797=CARTESIAN_POINT('Ctrl Pts',(12.985562223504,8.64349423686535,0.220119672968612));
#13798=CARTESIAN_POINT('Ctrl Pts',(12.7679935470831,10.9557088479816,0.108978525439593));
#13799=CARTESIAN_POINT('Ctrl Pts',(14.592171500868,12.3957303731543,-0.00216262208942797));
#13800=CARTESIAN_POINT('Ctrl Pts',(16.7924309645196,11.6375318213583,-0.113303769618446));
#13801=CARTESIAN_POINT('Ctrl Pts',(17.160799328377,10.1407345153594,-0.187397867971127));
#13802=CARTESIAN_POINT('Ctrl Pts',(16.9877912008532,9.47972727890995,-0.224444917147467));
#13803=CARTESIAN_POINT('Ctrl Pts',(14.5032651029123,8.14002119999724,8.07481497238249));
#13804=CARTESIAN_POINT('Ctrl Pts',(13.8847597760366,8.30520221168044,8.03776792320615));
#13805=CARTESIAN_POINT('Ctrl Pts',(12.8362023694098,9.29836719673542,7.96367382485347));
#13806=CARTESIAN_POINT('Ctrl Pts',(13.2375357061529,11.4415786404201,7.85253267732445));
#13807=CARTESIAN_POINT('Ctrl Pts',(15.2551626777114,12.2605314066992,7.74139152979544));
#13808=CARTESIAN_POINT('Ctrl Pts',(17.0377080509797,11.012593221171,7.63025038226641));
#13809=CARTESIAN_POINT('Ctrl Pts',(16.955794810566,8.83658643923375,7.51910923473739));
#13810=CARTESIAN_POINT('Ctrl Pts',(15.0832227804868,7.7261306463247,7.40796808720837));
#13811=CARTESIAN_POINT('Ctrl Pts',(13.1346790922697,8.69677120358184,7.29682693967935));
#13812=CARTESIAN_POINT('Ctrl Pts',(12.8934695001639,10.8604977819634,7.18568579215033));
#13813=CARTESIAN_POINT('Ctrl Pts',(14.5805498186396,12.2364751599715,7.07454464462132));
#13814=CARTESIAN_POINT('Ctrl Pts',(16.6515497766613,11.5653147145716,6.96340349709228));
#13815=CARTESIAN_POINT('Ctrl Pts',(17.2108010582909,9.46130481449049,6.85226234956328));
#13816=CARTESIAN_POINT('Ctrl Pts',(15.7463648741197,7.85040667225349,6.74112120203425));
#13817=CARTESIAN_POINT('Ctrl Pts',(13.5987397055133,8.2071553505388,6.62998005450523));
#13818=CARTESIAN_POINT('Ctrl Pts',(12.7337707910827,10.2050061974197,6.51883890697622));
#13819=CARTESIAN_POINT('Ctrl Pts',(13.94321953943,12.0152008981395,6.40769775944718));
#13820=CARTESIAN_POINT('Ctrl Pts',(16.1200028029027,11.9807611837112,6.29655661191817));
#13821=CARTESIAN_POINT('Ctrl Pts',(17.2715800583576,10.1332105724332,6.18541546438915));
#13822=CARTESIAN_POINT('Ctrl Pts',(16.3438425939259,8.16372448662726,6.07427431686013));
#13823=CARTESIAN_POINT('Ctrl Pts',(14.1860048228349,7.87509229519298,5.96313316933112));
#13824=CARTESIAN_POINT('Ctrl Pts',(12.7732660168176,9.53151666455001,5.85199202180209));
#13825=CARTESIAN_POINT('Ctrl Pts',(13.398791482955,11.6167721275012,5.74085087427307));
#13826=CARTESIAN_POINT('Ctrl Pts',(15.4899999103595,12.2220983207182,5.62970972674405));
#13827=CARTESIAN_POINT('Ctrl Pts',(17.132681797607,10.7934035556714,5.51856857921503));
#13828=CARTESIAN_POINT('Ctrl Pts',(16.823191081925,8.63845854771295,5.40742743168601));
#13829=CARTESIAN_POINT('Ctrl Pts',(14.8448233325836,7.72981475341796,5.296286284157));
#13830=CARTESIAN_POINT('Ctrl Pts',(13.0084981688392,8.8992087813196,5.18514513662797));
#13831=CARTESIAN_POINT('Ctrl Pts',(12.9951150460706,11.0762235695643,5.07400398909895));
#13832=CARTESIAN_POINT('Ctrl Pts',(14.8169243451838,12.2681058518924,4.96286284156994));
#13833=CARTESIAN_POINT('Ctrl Pts',(16.8063138607702,11.3838537086533,4.85172169404091));
#13834=CARTESIAN_POINT('Ctrl Pts',(17.1422750822405,9.23287659236945,4.7405805465119));
#13835=CARTESIAN_POINT('Ctrl Pts',(15.5172823900376,7.78409391454438,4.62943939898287));
#13836=CARTESIAN_POINT('Ctrl Pts',(13.4187898491597,8.3636640597211,4.51829825145385));
#13837=CARTESIAN_POINT('Ctrl Pts',(12.7676745659418,10.4410714307495,4.40715710392483));
#13838=CARTESIAN_POINT('Ctrl Pts',(14.15994172826,12.1147394521922,4.29601595639582));
#13839=CARTESIAN_POINT('Ctrl Pts',(16.3211650201456,11.8526585870353,4.18487480886679));
#13840=CARTESIAN_POINT('Ctrl Pts',(17.2730460859198,9.89472729766818,4.07373366133777));
#13841=CARTESIAN_POINT('Ctrl Pts',(16.1442706313649,8.033158477973,3.96259251380876));
#13842=CARTESIAN_POINT('Ctrl Pts',(13.9680750805259,7.97195862686682,3.85145136627974));
#13843=CARTESIAN_POINT('Ctrl Pts',(12.7364628029851,9.76714766846464,3.74031021875072));
#13844=CARTESIAN_POINT('Ctrl Pts',(13.5768029848114,11.7754805283458,3.62916907122169));
#13845=CARTESIAN_POINT('Ctrl Pts',(15.7198814470942,12.1586087076392,3.51802792369268));
#13846=CARTESIAN_POINT('Ctrl Pts',(17.2040088938011,10.5658318183123,3.40688677616365));
#13847=CARTESIAN_POINT('Ctrl Pts',(16.670673736408,8.45511485311085,3.29574562863464));
#13848=CARTESIAN_POINT('Ctrl Pts',(14.6080698921375,7.75852467310611,3.18460448110562));
#13849=CARTESIAN_POINT('Ctrl Pts',(12.9042233733512,9.11369238875171,3.0734633335766));
#13850=CARTESIAN_POINT('Ctrl Pts',(13.1187679203279,11.2801510509262,2.96232218604758));
#13851=CARTESIAN_POINT('Ctrl Pts',(15.0553179370813,12.274810052733,2.85118103851855));
#13852=CARTESIAN_POINT('Ctrl Pts',(16.9412321011123,11.1871978690395,2.74003989098954));
#13853=CARTESIAN_POINT('Ctrl Pts',(17.0502191482768,9.01287169225666,2.62889874346052));
#13854=CARTESIAN_POINT('Ctrl Pts',(15.2825166435939,7.7421237426291,2.5177575959315));
#13855=CARTESIAN_POINT('Ctrl Pts',(13.2562095740377,8.53814644977055,2.40661644840248));
#13856=CARTESIAN_POINT('Ctrl Pts',(12.8260993160138,10.6722921056024,2.29547530087346));
#13857=CARTESIAN_POINT('Ctrl Pts',(14.3858918014937,12.191048139099,2.18433415334444));
#13858=CARTESIAN_POINT('Ctrl Pts',(16.5078146442685,11.7042053473638,2.07319300581542));
#13859=CARTESIAN_POINT('Ctrl Pts',(17.2495435905392,9.65740032594834,1.9620518582864));
#13860=CARTESIAN_POINT('Ctrl Pts',(15.9321292402005,7.92419756291088,1.85091071075738));
#13861=CARTESIAN_POINT('Ctrl Pts',(13.7614806966379,8.09110216267724,1.73976956322836));
#13862=CARTESIAN_POINT('Ctrl Pts',(12.7245236397496,10.0053366046107,1.62862841569934));
#13863=CARTESIAN_POINT('Ctrl Pts',(13.7704479084177,11.9146856806772,1.51748726817032));
#13864=CARTESIAN_POINT('Ctrl Pts',(15.9418551082072,12.0714080533479,1.4063461206413));
#13865=CARTESIAN_POINT('Ctrl Pts',(17.2511262357788,10.332043702839,1.29520497311228));
#13866=CARTESIAN_POINT('Ctrl Pts',(16.4998037468857,8.28874294133233,1.18406382558326));
#13867=CARTESIAN_POINT('Ctrl Pts',(14.3756234213931,7.81185290478036,1.07292267805424));
#13868=CARTESIAN_POINT('Ctrl Pts',(12.8229664962652,9.33791847627317,0.961781530525221));
#13869=CARTESIAN_POINT('Ctrl Pts',(13.2630920505954,11.4700035275835,0.850640382996202));
#13870=CARTESIAN_POINT('Ctrl Pts',(15.2930910617157,12.2565515303325,0.739499235467181));
#13871=CARTESIAN_POINT('Ctrl Pts',(17.0548514658741,10.9774522176682,0.628358087938162));
#13872=CARTESIAN_POINT('Ctrl Pts',(16.9355941731834,8.80380475443427,0.517216940409142));
#13873=CARTESIAN_POINT('Ctrl Pts',(15.0447408557051,7.72477194324555,0.406075792880122));
#13874=CARTESIAN_POINT('Ctrl Pts',(13.1126032561702,8.72904261913709,0.294934645351101));
#13875=CARTESIAN_POINT('Ctrl Pts',(12.9087556038737,10.8954368254885,0.183793497822082));
#13876=CARTESIAN_POINT('Ctrl Pts',(14.6178913092855,12.2446430255347,0.0726523502930609));
#13877=CARTESIAN_POINT('Ctrl Pts',(16.6793908481296,11.5342604589779,-0.0384887972359571));
#13878=CARTESIAN_POINT('Ctrl Pts',(17.0245279670748,10.1318590572183,-0.112582895588638));
#13879=CARTESIAN_POINT('Ctrl Pts',(16.8624306412829,9.51253841089255,-0.149629944764978));
#13880=CARTESIAN_POINT('Ctrl Pts',(14.5367004230132,8.26521672566619,8.14962994476498));
#13881=CARTESIAN_POINT('Ctrl Pts',(13.9598268069544,8.41927937213568,8.11258289558864));
#13882=CARTESIAN_POINT('Ctrl Pts',(12.9818479981678,9.34559423374852,8.03848879723595));
#13883=CARTESIAN_POINT('Ctrl Pts',(13.3561675119244,11.3445457088188,7.92734764970695));
#13884=CARTESIAN_POINT('Ctrl Pts',(15.2379876294974,12.1083746091312,7.81620650217792));
#13885=CARTESIAN_POINT('Ctrl Pts',(16.9005495357311,10.9444353794724,7.7050653546489));
#13886=CARTESIAN_POINT('Ctrl Pts',(16.8241498910599,8.91489602658511,7.59392420711988));
#13887=CARTESIAN_POINT('Ctrl Pts',(15.0776210393537,7.87918522363254,7.48278305959087));
#13888=CARTESIAN_POINT('Ctrl Pts',(13.2602341962226,8.78449178095305,7.37164191206184));
#13889=CARTESIAN_POINT('Ctrl Pts',(13.0352604674934,10.8025775131143,7.26050076453282));
#13890=CARTESIAN_POINT('Ctrl Pts',(14.6087830898722,12.0859375929316,7.1493596170038));
#13891=CARTESIAN_POINT('Ctrl Pts',(16.5403836480704,11.4599530843595,7.03821846947479));
#13892=CARTESIAN_POINT('Ctrl Pts',(17.0619916199027,9.49756448956049,6.92707732194575));
#13893=CARTESIAN_POINT('Ctrl Pts',(15.6961269129365,7.99509620669406,6.81593617441675));
#13894=CARTESIAN_POINT('Ctrl Pts',(13.6930588016057,8.32783206380658,6.70479502688771));
#13895=CARTESIAN_POINT('Ctrl Pts',(12.8863111087983,10.1912071914035,6.59365387935871));
#13896=CARTESIAN_POINT('Ctrl Pts',(14.0143516325902,11.8795573436157,6.48251273182967));
#13897=CARTESIAN_POINT('Ctrl Pts',(16.0446152018935,11.8474357728952,6.37137158430067));
#13898=CARTESIAN_POINT('Ctrl Pts',(17.1186795739517,10.1242441435468,6.26023043677163));
#13899=CARTESIAN_POINT('Ctrl Pts',(16.2533882941443,8.28732453957915,6.14908928924263));
#13900=CARTESIAN_POINT('Ctrl Pts',(14.2407949925385,8.01812023567324,6.0379481417136));
#13901=CARTESIAN_POINT('Ctrl Pts',(12.9231479034009,9.56305036668077,5.92680699418458));
#13902=CARTESIAN_POINT('Ctrl Pts',(13.5065691318168,11.5079468890688,5.81566584665556));
#13903=CARTESIAN_POINT('Ctrl Pts',(15.4570179234921,12.0725284614542,5.70452469912655));
#13904=CARTESIAN_POINT('Ctrl Pts',(16.9891305814665,10.7399994119146,5.59338355159752));
#13905=CARTESIAN_POINT('Ctrl Pts',(16.7004717445346,8.73010416100646,5.4822424040685));
#13906=CARTESIAN_POINT('Ctrl Pts',(14.8552683034879,7.88262135277884,5.37110125653948));
#13907=CARTESIAN_POINT('Ctrl Pts',(13.1425465346714,8.97330324695236,5.25996010901047));
#13908=CARTESIAN_POINT('Ctrl Pts',(13.1300642324337,11.0037827570514,5.14881896148144));
#13909=CARTESIAN_POINT('Ctrl Pts',(14.8292472022195,12.1154392169823,5.03767781395242));
#13910=CARTESIAN_POINT('Ctrl Pts',(16.6847305323356,11.2907062531535,4.92653666642341));
#13911=CARTESIAN_POINT('Ctrl Pts',(16.9980781402925,9.28451181437904,4.81539551889438));
#13912=CARTESIAN_POINT('Ctrl Pts',(15.4824640142906,7.93324697327884,4.70425437136536));
#13913=CARTESIAN_POINT('Ctrl Pts',(13.5252214042007,8.4738061421007,4.59311322383634));
#13914=CARTESIAN_POINT('Ctrl Pts',(12.9179328141437,10.4113828291212,4.48197207630733));
#13915=CARTESIAN_POINT('Ctrl Pts',(14.2164862098008,11.9723959387232,4.3708309287783));
#13916=CARTESIAN_POINT('Ctrl Pts',(16.2322371521546,11.727955786289,4.25968978124929));
#13917=CARTESIAN_POINT('Ctrl Pts',(17.1200469229207,9.90181322322121,4.14854863372026));
#13918=CARTESIAN_POINT('Ctrl Pts',(16.0672495582209,8.16554695372194,4.03740748619125));
#13919=CARTESIAN_POINT('Ctrl Pts',(14.0375341425024,8.10846647619684,3.92626633866222));
#13920=CARTESIAN_POINT('Ctrl Pts',(12.8888219208692,9.78282100304769,3.81512519113321));
#13921=CARTESIAN_POINT('Ctrl Pts',(13.6725986457333,11.6559725973624,3.70398404360418));
#13922=CARTESIAN_POINT('Ctrl Pts',(15.6714260904051,12.0133123462689,3.59284289607517));
#13923=CARTESIAN_POINT('Ctrl Pts',(17.0556566372925,10.5277455713434,3.48170174854614));
#13924=CARTESIAN_POINT('Ctrl Pts',(16.5582203704607,8.55910136524887,3.37056060101713));
#13925=CARTESIAN_POINT('Ctrl Pts',(14.6344507820053,7.90939880232955,3.2594194534881));
#13926=CARTESIAN_POINT('Ctrl Pts',(13.0452904954375,9.17334992210343,3.14827830595909));
#13927=CARTESIAN_POINT('Ctrl Pts',(13.2453940082809,11.1939838409794,3.03713715843007));
#13928=CARTESIAN_POINT('Ctrl Pts',(15.0515944762484,12.1216921567933,2.92599601090104));
#13929=CARTESIAN_POINT('Ctrl Pts',(16.8105674003405,11.1072873553889,2.81485486337203));
#13930=CARTESIAN_POINT('Ctrl Pts',(16.9122185086971,9.07931548580447,2.703713715843));
#13931=CARTESIAN_POINT('Ctrl Pts',(15.2635003947501,7.89410182159245,2.59257256831399));
#13932=CARTESIAN_POINT('Ctrl Pts',(13.3735844382213,8.63654408939513,2.48143142078496));
#13933=CARTESIAN_POINT('Ctrl Pts',(12.9724249832114,10.6270399965118,2.37029027325595));
#13934=CARTESIAN_POINT('Ctrl Pts',(14.4272275407664,12.0435682734467,2.25914912572692));
#13935=CARTESIAN_POINT('Ctrl Pts',(16.4063233546902,11.5894949623257,2.14800797819791));
#13936=CARTESIAN_POINT('Ctrl Pts',(17.0981263849601,9.6804607749636,2.03686683066889));
#13937=CARTESIAN_POINT('Ctrl Pts',(15.8693874443165,8.06392021851098,1.92572568313987));
#13938=CARTESIAN_POINT('Ctrl Pts',(13.844845665763,8.21959043802295,1.81458453561085));
#13939=CARTESIAN_POINT('Ctrl Pts',(12.8776863849747,10.0049773967426,1.70344338808183));
#13940=CARTESIAN_POINT('Ctrl Pts',(13.8532092928178,11.7858078244979,1.59230224055281));
#13941=CARTESIAN_POINT('Ctrl Pts',(15.8784586623037,11.9319811845506,1.48116109302379));
#13942=CARTESIAN_POINT('Ctrl Pts',(17.0996025020485,10.3096937782474,1.37001994549477));
#13943=CARTESIAN_POINT('Ctrl Pts',(16.398851672329,8.40392797839529,1.25887879796575));
#13944=CARTESIAN_POINT('Ctrl Pts',(14.4176503272771,7.95913750061909,1.14773765043673));
#13945=CARTESIAN_POINT('Ctrl Pts',(12.969503034154,9.3824833091619,1.03659650290771));
#13946=CARTESIAN_POINT('Ctrl Pts',(13.3800036539771,11.371057311438,0.92545535537869));
#13947=CARTESIAN_POINT('Ctrl Pts',(15.2733630467833,12.1046626189973,0.814314207849671));
#13948=CARTESIAN_POINT('Ctrl Pts',(16.9165390241187,10.9116597235779,0.70317306032065));
#13949=CARTESIAN_POINT('Ctrl Pts',(16.8053089624094,8.88432088320471,0.592031912791632));
#13950=CARTESIAN_POINT('Ctrl Pts',(15.041729340225,7.87791797511523,0.480890765262611));
#13951=CARTESIAN_POINT('Ctrl Pts',(13.2396442888365,8.81459100140882,0.36974961773359));
#13952=CARTESIAN_POINT('Ctrl Pts',(13.0495176606643,10.8351648029955,0.258608470204571));
#13953=CARTESIAN_POINT('Ctrl Pts',(14.643611117703,12.0935556779152,0.14746732267555));
#13954=CARTESIAN_POINT('Ctrl Pts',(16.5663507317396,11.4309890965976,0.0363261751465319));
#13955=CARTESIAN_POINT('Ctrl Pts',(16.8882566057727,10.1229835990773,-0.0377679232061492));
#13956=CARTESIAN_POINT('Ctrl Pts',(16.7370700817125,9.54534954287515,-0.0748149723824891));
#13957=CARTESIAN_POINT('Ctrl Pts',(14.5701357431141,8.39041225133515,8.22444491714747));
#13958=CARTESIAN_POINT('Ctrl Pts',(14.0348938378722,8.53335653259092,8.18739786797113));
#13959=CARTESIAN_POINT('Ctrl Pts',(13.1274936269258,9.39282127076158,8.11330376961845));
#13960=CARTESIAN_POINT('Ctrl Pts',(13.4747993176958,11.2475127772175,8.00216262208943));
#13961=CARTESIAN_POINT('Ctrl Pts',(15.2208125812833,11.9562178115631,7.89102147456041));
#13962=CARTESIAN_POINT('Ctrl Pts',(16.7633910204825,10.8762775377738,7.77988032703138));
#13963=CARTESIAN_POINT('Ctrl Pts',(16.6925049715538,8.99320561393648,7.66873917950237));
#13964=CARTESIAN_POINT('Ctrl Pts',(15.0720192982206,8.03223980094035,7.55759803197335));
#13965=CARTESIAN_POINT('Ctrl Pts',(13.3857893001755,8.87221235832429,7.44645688444433));
#13966=CARTESIAN_POINT('Ctrl Pts',(13.1770514348228,10.7446572442652,7.33531573691531));
#13967=CARTESIAN_POINT('Ctrl Pts',(14.6370163611048,11.9354000258917,7.22417458938629));
#13968=CARTESIAN_POINT('Ctrl Pts',(16.4292175194794,11.3545914541475,7.11303344185728));
#13969=CARTESIAN_POINT('Ctrl Pts',(16.9131821815146,9.53382416463051,7.00189229432824));
#13970=CARTESIAN_POINT('Ctrl Pts',(15.6458889517532,8.1397857411346,6.89075114679924));
#13971=CARTESIAN_POINT('Ctrl Pts',(13.7873778976981,8.44850877707437,6.7796099992702));
#13972=CARTESIAN_POINT('Ctrl Pts',(13.0388514265139,10.1774081853872,6.6684688517412));
#13973=CARTESIAN_POINT('Ctrl Pts',(14.0854837257504,11.743913789092,6.55732770421216));
#13974=CARTESIAN_POINT('Ctrl Pts',(15.9692276008844,11.7141103620792,6.44618655668316));
#13975=CARTESIAN_POINT('Ctrl Pts',(16.9657790895458,10.1152777146604,6.33504540915412));
#13976=CARTESIAN_POINT('Ctrl Pts',(16.1629339943627,8.41092459253105,6.22390426162512));
#13977=CARTESIAN_POINT('Ctrl Pts',(14.295585162242,8.16114817615349,6.11276311409608));
#13978=CARTESIAN_POINT('Ctrl Pts',(13.0730297899843,9.59458406881153,6.00162196656708));
#13979=CARTESIAN_POINT('Ctrl Pts',(13.6143467806786,11.3991216506364,5.89048081903804));
#13980=CARTESIAN_POINT('Ctrl Pts',(15.4240359366248,11.9229586021902,5.77933967150904));
#13981=CARTESIAN_POINT('Ctrl Pts',(16.8455793653259,10.6865952681579,5.66819852398001));
#13982=CARTESIAN_POINT('Ctrl Pts',(16.5777524071442,8.82174977429995,5.55705737645099));
#13983=CARTESIAN_POINT('Ctrl Pts',(14.8657132743923,8.03542795213972,5.44591622892198));
#13984=CARTESIAN_POINT('Ctrl Pts',(13.2765949005036,9.04739771258512,5.33477508139295));
#13985=CARTESIAN_POINT('Ctrl Pts',(13.2650134187968,10.9313419445386,5.22363393386393));
#13986=CARTESIAN_POINT('Ctrl Pts',(14.8415700592552,11.9627725820722,5.11249278633491));
#13987=CARTESIAN_POINT('Ctrl Pts',(16.5631472039009,11.1975587976537,5.0013516388059));
#13988=CARTESIAN_POINT('Ctrl Pts',(16.8538811983444,9.33614703638862,4.89021049127687));
#13989=CARTESIAN_POINT('Ctrl Pts',(15.4476456385435,8.08240003201331,4.77906934374786));
#13990=CARTESIAN_POINT('Ctrl Pts',(13.6316529592416,8.58394822448031,4.66792819621882));
#13991=CARTESIAN_POINT('Ctrl Pts',(13.0681910623456,10.381694227493,4.55678704868982));
#13992=CARTESIAN_POINT('Ctrl Pts',(14.2730306913416,11.8300524252543,4.44564590116079));
#13993=CARTESIAN_POINT('Ctrl Pts',(16.1433092841637,11.6032529855428,4.33450475363178));
#13994=CARTESIAN_POINT('Ctrl Pts',(16.9670477599216,9.90889914877423,4.22336360610275));
#13995=CARTESIAN_POINT('Ctrl Pts',(15.9902284850769,8.29793542947089,4.11222245857374));
#13996=CARTESIAN_POINT('Ctrl Pts',(14.106993204479,8.24497432552685,4.00108131104471));
#13997=CARTESIAN_POINT('Ctrl Pts',(13.0411810387533,9.79849433763074,3.8899401635157));
#13998=CARTESIAN_POINT('Ctrl Pts',(13.7683943066552,11.536464666379,3.77879901598667));
#13999=CARTESIAN_POINT('Ctrl Pts',(15.622970733716,11.8680159848985,3.66765786845765));
#14000=CARTESIAN_POINT('Ctrl Pts',(16.907304380784,10.4896593243745,3.55651672092864));
#14001=CARTESIAN_POINT('Ctrl Pts',(16.4457670045134,8.66308787738691,3.44537557339961));
#14002=CARTESIAN_POINT('Ctrl Pts',(14.6608316718731,8.06027293155299,3.3342344258706));
#14003=CARTESIAN_POINT('Ctrl Pts',(13.1863576175239,9.23300745545514,3.22309327834157));
#14004=CARTESIAN_POINT('Ctrl Pts',(13.3720200962339,11.1078166310327,3.11195213081256));
#14005=CARTESIAN_POINT('Ctrl Pts',(15.0478710154155,11.9685742608536,3.00081098328353));
#14006=CARTESIAN_POINT('Ctrl Pts',(16.6799026995687,11.0273768417383,2.88966983575452));
#14007=CARTESIAN_POINT('Ctrl Pts',(16.7742178691174,9.14575927935223,2.77852868822549));
#14008=CARTESIAN_POINT('Ctrl Pts',(15.2444841459064,8.04607990055583,2.66738754069648));
#14009=CARTESIAN_POINT('Ctrl Pts',(13.490959302405,8.73494172901969,2.55624639316745));
#14010=CARTESIAN_POINT('Ctrl Pts',(13.118750650409,10.5817878874212,2.44510524563844));
#14011=CARTESIAN_POINT('Ctrl Pts',(14.468563280039,11.8960884077944,2.33396409810942));
#14012=CARTESIAN_POINT('Ctrl Pts',(16.304832065112,11.4747845772875,2.2228229505804));
#14013=CARTESIAN_POINT('Ctrl Pts',(16.946709179381,9.70352122397884,2.11168180305138));
#14014=CARTESIAN_POINT('Ctrl Pts',(15.8066456484325,8.20364287411109,2.00054065552236));
#14015=CARTESIAN_POINT('Ctrl Pts',(13.9282106348881,8.34807871336868,1.88939950799334));
#14016=CARTESIAN_POINT('Ctrl Pts',(13.0308491301998,10.0046181888745,1.77825836046432));
#14017=CARTESIAN_POINT('Ctrl Pts',(13.9359706772179,11.6569299683187,1.6671172129353));
#14018=CARTESIAN_POINT('Ctrl Pts',(15.8150622164002,11.7925543157533,1.55597606540628));
#14019=CARTESIAN_POINT('Ctrl Pts',(16.9480787683183,10.2873438536559,1.44483491787726));
#14020=CARTESIAN_POINT('Ctrl Pts',(16.2978995977724,8.51911301545824,1.33369377034824));
#14021=CARTESIAN_POINT('Ctrl Pts',(14.4596772331612,8.10642209645783,1.22255262281922));
#14022=CARTESIAN_POINT('Ctrl Pts',(13.1160395720428,9.42704814205063,1.1114114752902));
#14023=CARTESIAN_POINT('Ctrl Pts',(13.4969152573589,11.2721110952926,1.00027032776118));
#14024=CARTESIAN_POINT('Ctrl Pts',(15.2536350318509,11.952773707662,0.88912918023216));
#14025=CARTESIAN_POINT('Ctrl Pts',(16.7782265823633,10.8458672294876,0.777988032703139));
#14026=CARTESIAN_POINT('Ctrl Pts',(16.6750237516355,8.96483701197515,0.666846885174121));
#14027=CARTESIAN_POINT('Ctrl Pts',(15.0387178247449,8.0310640069849,0.555705737645099));
#14028=CARTESIAN_POINT('Ctrl Pts',(13.3666853215027,8.90013938368058,0.44456459011608));
#14029=CARTESIAN_POINT('Ctrl Pts',(13.1902797174549,10.7748927805024,0.33342344258706));
#14030=CARTESIAN_POINT('Ctrl Pts',(14.6693309261205,11.9424683302957,0.222282295058039));
#14031=CARTESIAN_POINT('Ctrl Pts',(16.4533106153496,11.3277177342173,0.111141147529021));
#14032=CARTESIAN_POINT('Ctrl Pts',(16.7519852444706,10.1141081409362,0.0370470491763399));
#14033=CARTESIAN_POINT('Ctrl Pts',(16.6117095221421,9.57816067485776,0.));
#14034=CARTESIAN_POINT('Ctrl Pts',(13.3361815072522,10.0009395500142,7.3785196366098));
#14035=CARTESIAN_POINT('Ctrl Pts',(13.3350652939176,10.2169537828321,7.36411833671163));
#14036=CARTESIAN_POINT('Ctrl Pts',(13.3741036482068,10.4325813967082,7.34971703681347));
#14037=CARTESIAN_POINT('Ctrl Pts',(13.4551685667619,10.6310402268794,7.33531573691531));
#14038=CARTESIAN_POINT('Ctrl Pts',(13.6637064102501,11.1415715048073,7.29826868773897));
#14039=CARTESIAN_POINT('Ctrl Pts',(14.1503613856775,11.5384857653495,7.26122163856263));
#14040=CARTESIAN_POINT('Ctrl Pts',(14.6923890664536,11.6401414669966,7.22417458938629));
#14041=CARTESIAN_POINT('Ctrl Pts',(15.2344167472297,11.7417971686436,7.18712754020995));
#14042=CARTESIAN_POINT('Ctrl Pts',(15.8318171333545,11.5481943113955,7.15008049103361));
#14043=CARTESIAN_POINT('Ctrl Pts',(16.2111781034228,11.147931667852,7.11303344185727));
#14044=CARTESIAN_POINT('Ctrl Pts',(16.5905390734911,10.7476690243085,7.07598639268093));
#14045=CARTESIAN_POINT('Ctrl Pts',(16.7518606275029,10.1407465944695,7.03893934350459));
#14046=CARTESIAN_POINT('Ctrl Pts',(16.6213058662152,9.60494564230069,7.00189229432825));
#14047=CARTESIAN_POINT('Ctrl Pts',(16.4907511049275,9.06914469013187,6.9648452451519));
#14048=CARTESIAN_POINT('Ctrl Pts',(16.0683200283403,8.60446521563324,6.92779819597557));
#14049=CARTESIAN_POINT('Ctrl Pts',(15.5473526477042,8.42357931770721,6.89075114679923));
#14050=CARTESIAN_POINT('Ctrl Pts',(15.0263852670682,8.24269341978119,6.85370409762289));
#14051=CARTESIAN_POINT('Ctrl Pts',(14.4068815823831,8.34560109842778,6.81665704844655));
#14052=CARTESIAN_POINT('Ctrl Pts',(13.9723753281766,8.68520483913655,6.77960999927021));
#14053=CARTESIAN_POINT('Ctrl Pts',(13.5771626118018,8.99409732470422,6.74591321171674));
#14054=CARTESIAN_POINT('Ctrl Pts',(13.3350006419844,9.49881149769819,6.71221642416327));
#14055=CARTESIAN_POINT('Ctrl Pts',(13.3318213113649,10.0008675364682,6.6785196366098));
#14056=CARTESIAN_POINT('Ctrl Pts',(14.4698297828114,8.01482567432828,8.));
#14057=CARTESIAN_POINT('Ctrl Pts',(14.3998214936988,8.04074714826579,8.));
#14058=CARTESIAN_POINT('Ctrl Pts',(14.3314995809058,8.07074117787574,8.));
#14059=CARTESIAN_POINT('Ctrl Pts',(14.2650833692488,8.10452090745416,8.));
#14060=CARTESIAN_POINT('Ctrl Pts',(14.2004102705822,8.13741407810413,8.));
#14061=CARTESIAN_POINT('Ctrl Pts',(14.1375437306998,8.1738977671453,8.));
#14062=CARTESIAN_POINT('Ctrl Pts',(14.0767171887106,8.21374090711945,8.));
#14063=CARTESIAN_POINT('Ctrl Pts',(14.0631405149643,8.22263402013834,8.));
#14064=CARTESIAN_POINT('Ctrl Pts',(14.0496638268926,8.23169584191256,8.));
#14065=CARTESIAN_POINT('Ctrl Pts',(14.036295680768,8.240920018892,8.));
#14066=CARTESIAN_POINT('Ctrl Pts',(13.9749539654965,8.28324651896258,8.));
#14067=CARTESIAN_POINT('Ctrl Pts',(13.9160153999523,8.32890389170504,8.));
#14068=CARTESIAN_POINT('Ctrl Pts',(13.8597185778864,8.37762279724655,8.));
#14069=CARTESIAN_POINT('Ctrl Pts',(13.8201934931154,8.41182754985629,8.));
#14070=CARTESIAN_POINT('Ctrl Pts',(13.7819713009793,8.44754226231406,8.));
#14071=CARTESIAN_POINT('Ctrl Pts',(13.7451474325163,8.48468212230948,8.));
#14072=CARTESIAN_POINT('Ctrl Pts',(13.7311387285853,8.49881103717989,8.));
#14073=CARTESIAN_POINT('Ctrl Pts',(13.7173325138727,8.51314626010991,8.));
#14074=CARTESIAN_POINT('Ctrl Pts',(13.7037345023968,8.52768330428626,8.));
#14075=CARTESIAN_POINT('Ctrl Pts',(13.6908096643821,8.54150068791797,8.));
#14076=CARTESIAN_POINT('Ctrl Pts',(13.6780691038482,8.55550494493883,8.));
#14077=CARTESIAN_POINT('Ctrl Pts',(13.6655397272255,8.56966702391835,8.));
#14078=CARTESIAN_POINT('Ctrl Pts',(13.6174406383793,8.62403390230305,8.));
#14079=CARTESIAN_POINT('Ctrl Pts',(13.5723959858275,8.68077902345639,8.));
#14080=CARTESIAN_POINT('Ctrl Pts',(13.5306283225234,8.73965444066073,8.));
#14081=CARTESIAN_POINT('Ctrl Pts',(13.4897585658688,8.79726417469265,8.));
#14082=CARTESIAN_POINT('Ctrl Pts',(13.4520260621303,8.85691446263185,8.));
#14083=CARTESIAN_POINT('Ctrl Pts',(13.4176844468098,8.91839214182768,8.));
#14084=CARTESIAN_POINT('Ctrl Pts',(13.3840956014734,8.97852222711571,8.));
#14085=CARTESIAN_POINT('Ctrl Pts',(13.3537503389223,9.0404011858163,8.));
#14086=CARTESIAN_POINT('Ctrl Pts',(13.3269342184203,9.10383656685819,8.));
#14087=CARTESIAN_POINT('Ctrl Pts',(13.318222609287,9.12444447861096,8.));
#14088=CARTESIAN_POINT('Ctrl Pts',(13.3098838590006,9.1452166622322,8.));
#14089=CARTESIAN_POINT('Ctrl Pts',(13.3019289624212,9.16614649473232,8.));
#14090=CARTESIAN_POINT('Ctrl Pts',(13.2974345589444,9.17797155254661,8.));
#14091=CARTESIAN_POINT('Ctrl Pts',(13.2930623430191,9.18984821638012,8.));
#14092=CARTESIAN_POINT('Ctrl Pts',(13.2888201205526,9.20175830442571,8.));
#14093=CARTESIAN_POINT('Ctrl Pts',(13.2659037845155,9.26609617968757,8.));
#14094=CARTESIAN_POINT('Ctrl Pts',(13.2467332556311,9.3315197201952,8.));
#14095=CARTESIAN_POINT('Ctrl Pts',(13.2315368288626,9.39782942737589,8.));
#14096=CARTESIAN_POINT('Ctrl Pts',(13.2293394455293,9.40741772386231,8.));
#14097=CARTESIAN_POINT('Ctrl Pts',(13.2272252438361,9.41702456272481,8.));
#14098=CARTESIAN_POINT('Ctrl Pts',(13.2251950049826,9.42664935181928,8.));
#14099=CARTESIAN_POINT('Ctrl Pts',(13.2108763834671,9.49452989305377,8.));
#14100=CARTESIAN_POINT('Ctrl Pts',(13.2007298389188,9.56330380603441,8.));
#14101=CARTESIAN_POINT('Ctrl Pts',(13.1946587081026,9.63261524468971,8.));
#14102=CARTESIAN_POINT('Ctrl Pts',(13.1889946919687,9.69727883351621,8.));
#14103=CARTESIAN_POINT('Ctrl Pts',(13.1868786273274,9.76241098193826,8.));
#14104=CARTESIAN_POINT('Ctrl Pts',(13.1882701725515,9.82771039931623,8.));
#14105=CARTESIAN_POINT('Ctrl Pts',(13.1885789791415,9.84220140547489,8.));
#14106=CARTESIAN_POINT('Ctrl Pts',(13.1890606579093,9.85670057589872,8.));
#14107=CARTESIAN_POINT('Ctrl Pts',(13.1897149907357,9.87120447799809,8.));
#14108=CARTESIAN_POINT('Ctrl Pts',(13.1902222155533,9.8824475928177,8.));
#14109=CARTESIAN_POINT('Ctrl Pts',(13.1908332280675,9.89369266287328,8.));
#14110=CARTESIAN_POINT('Ctrl Pts',(13.1915468679667,9.90492535693582,8.));
#14111=CARTESIAN_POINT('Ctrl Pts',(13.1958826255629,9.97317019394023,8.));
#14112=CARTESIAN_POINT('Ctrl Pts',(13.2040074350011,10.0410843826852,8.));
#14113=CARTESIAN_POINT('Ctrl Pts',(13.2158110352946,10.1083321091977,8.));
#14114=CARTESIAN_POINT('Ctrl Pts',(13.2275596947567,10.1752668256192,8.));
#14115=CARTESIAN_POINT('Ctrl Pts',(13.2429534648895,10.2415422967115,8.));
#14116=CARTESIAN_POINT('Ctrl Pts',(13.2619307505069,10.306807573732,8.));
#14117=CARTESIAN_POINT('Ctrl Pts',(13.2805005504678,10.3706714562232,8.));
#14118=CARTESIAN_POINT('Ctrl Pts',(13.3025021612721,10.4335688734512,8.));
#14119=CARTESIAN_POINT('Ctrl Pts',(13.3279154052132,10.4951385987467,8.));
#14120=CARTESIAN_POINT('Ctrl Pts',(13.3333017419517,10.5081883012605,8.));
#14121=CARTESIAN_POINT('Ctrl Pts',(13.3388414595185,10.5211782174638,8.));
#14122=CARTESIAN_POINT('Ctrl Pts',(13.344534554462,10.5341046634128,8.));
#14123=CARTESIAN_POINT('Ctrl Pts',(13.3498584076977,10.546192728301,8.));
#14124=CARTESIAN_POINT('Ctrl Pts',(13.3553171624044,10.5582266610946,8.));
#14125=CARTESIAN_POINT('Ctrl Pts',(13.3609016527936,10.5701845006962,8.));
#14126=CARTESIAN_POINT('Ctrl Pts',(13.3885543554232,10.6293960955872,8.));
#14127=CARTESIAN_POINT('Ctrl Pts',(13.419333021235,10.6868524927592,8.));
#14128=CARTESIAN_POINT('Ctrl Pts',(13.4531736194346,10.7422401797738,8.));
#14129=CARTESIAN_POINT('Ctrl Pts',(13.4863693140172,10.7965723381752,8.));
#14130=CARTESIAN_POINT('Ctrl Pts',(13.5225118662568,10.8489145978588,8.));
#14131=CARTESIAN_POINT('Ctrl Pts',(13.5615753972507,10.8989353051115,8.));
#14132=CARTESIAN_POINT('Ctrl Pts',(13.5993684169907,10.9473291273931,8.));
#14133=CARTESIAN_POINT('Ctrl Pts',(13.6398959829063,10.9935504147084,8.));
#14134=CARTESIAN_POINT('Ctrl Pts',(13.6831600007655,11.0372567515148,8.));
#14135=CARTESIAN_POINT('Ctrl Pts',(13.6903680308745,11.0445384744625,8.));
#14136=CARTESIAN_POINT('Ctrl Pts',(13.6976520674348,11.0517502824926,8.));
#14137=CARTESIAN_POINT('Ctrl Pts',(13.7050121765453,11.0588904602709,8.));
#14138=CARTESIAN_POINT('Ctrl Pts',(13.7127728136493,11.0664191976529,8.));
#14139=CARTESIAN_POINT('Ctrl Pts',(13.7206180292613,11.0738682961014,8.));
#14140=CARTESIAN_POINT('Ctrl Pts',(13.7285463279864,11.0812370110871,8.));
#14141=CARTESIAN_POINT('Origin',(-15.,10.,9.54592528053767));
#14142=CARTESIAN_POINT('Ctrl Pts',(-17.056546936061,10.0014880949897,7.79592528053768));
#14143=CARTESIAN_POINT('Ctrl Pts',(-17.0573685174097,10.0998546456676,7.79057696270225));
#14144=CARTESIAN_POINT('Ctrl Pts',(-17.0062396152572,10.8787654055349,7.74818159569048));
#14145=CARTESIAN_POINT('Ctrl Pts',(-16.0106087131083,12.2086083874229,7.66873917950237));
#14146=CARTESIAN_POINT('Ctrl Pts',(-13.6926512300581,12.0466287931598,7.55759803197335));
#14147=CARTESIAN_POINT('Ctrl Pts',(-12.5713806281451,10.011647112944,7.44645688444433));
#14148=CARTESIAN_POINT('Ctrl Pts',(-13.673176561786,7.96579721763555,7.33531573691531));
#14149=CARTESIAN_POINT('Ctrl Pts',(-15.989491953976,7.78208289239259,7.22417458938629));
#14150=CARTESIAN_POINT('Ctrl Pts',(-17.0022525717684,9.10777352753874,7.14437777059374));
#14151=CARTESIAN_POINT('Ctrl Pts',(-17.0572654529527,9.89346180187816,7.10162800097754));
#14152=CARTESIAN_POINT('Ctrl Pts',(-17.0563655762952,9.99839712210779,7.09592528053768));
#14153=CARTESIAN_POINT('Ctrl Pts',(-17.052688542414,9.99752997529134,7.85407471946233));
#14154=CARTESIAN_POINT('Ctrl Pts',(-17.0491243489968,10.4678340862227,7.82862238128887));
#14155=CARTESIAN_POINT('Ctrl Pts',(-16.6564410380322,11.6297982528173,7.76612299393908));
#14156=CARTESIAN_POINT('Ctrl Pts',(-14.7276622354211,12.4126888235087,7.66657655741294));
#14157=CARTESIAN_POINT('Ctrl Pts',(-12.8251333276493,11.0807508020576,7.55543540988392));
#14158=CARTESIAN_POINT('Ctrl Pts',(-12.9125602025977,8.75827697936691,7.4442942623549));
#14159=CARTESIAN_POINT('Ctrl Pts',(-14.9111754557965,7.5730758609676,7.33315311482589));
#14160=CARTESIAN_POINT('Ctrl Pts',(-16.7213954228828,8.4748124655939,7.23641326719502));
#14161=CARTESIAN_POINT('Ctrl Pts',(-17.0498947507887,9.58221923747805,7.1767204687405));
#14162=CARTESIAN_POINT('Ctrl Pts',(-17.0520595406494,10.0011587933795,7.15407471946232));
#14163=CARTESIAN_POINT('Ctrl Pts',(-13.7309291201476,11.0793586530485,8.));
#14164=CARTESIAN_POINT('Ctrl Pts',(-13.3720061708544,10.657350026192,7.96295295082366));
#14165=CARTESIAN_POINT('Ctrl Pts',(-13.114537813302,9.43433491073641,7.88885885247098));
#14166=CARTESIAN_POINT('Ctrl Pts',(-14.4551167789601,8.1064248597425,7.77771770494196));
#14167=CARTESIAN_POINT('Ctrl Pts',(-16.2942884601245,8.51663726829463,7.66657655741294));
#14168=CARTESIAN_POINT('Ctrl Pts',(-16.9487772812347,10.2822716397578,7.55543540988393));
#14169=CARTESIAN_POINT('Ctrl Pts',(-15.8194058235982,11.790749031973,7.4442942623549));
#14170=CARTESIAN_POINT('Ctrl Pts',(-13.9399960818965,11.659415291108,7.33315311482589));
#14171=CARTESIAN_POINT('Ctrl Pts',(-13.0308651303028,10.0094435284899,7.22201196729686));
#14172=CARTESIAN_POINT('Ctrl Pts',(-13.9242059384039,8.3506597710577,7.11087081976784));
#14173=CARTESIAN_POINT('Ctrl Pts',(-15.8022842658834,8.20170341828741,6.99972967223882));
#14174=CARTESIAN_POINT('Ctrl Pts',(-16.9459842407539,9.69879198933349,6.8885885247098));
#14175=CARTESIAN_POINT('Ctrl Pts',(-16.3084066898541,11.4716175152832,6.77744737718078));
#14176=CARTESIAN_POINT('Ctrl Pts',(-14.4731656357203,11.8973706549213,6.66630622965176));
#14177=CARTESIAN_POINT('Ctrl Pts',(-13.1201677999229,10.5863518488495,6.55516508212274));
#14178=CARTESIAN_POINT('Ctrl Pts',(-13.4878941064161,8.73860657507213,6.44402393459372));
#14179=CARTESIAN_POINT('Ctrl Pts',(-15.2397423309735,8.0454926065714,6.3328827870647));
#14180=CARTESIAN_POINT('Ctrl Pts',(-16.7721399220139,9.14145658964824,6.22174163953569));
#14181=CARTESIAN_POINT('Ctrl Pts',(-16.6823906822222,11.023297702524,6.11060049200666));
#14182=CARTESIAN_POINT('Ctrl Pts',(-15.0526475313575,11.9684523308575,5.99945934447764));
#14183=CARTESIAN_POINT('Ctrl Pts',(-13.3747129092986,11.111763635759,5.88831819694862));
#14184=CARTESIAN_POINT('Ctrl Pts',(-13.1845018342894,9.23741040317065,5.77717704941961));
#14185=CARTESIAN_POINT('Ctrl Pts',(-14.6561260023258,8.06110156877586,5.66603590189058));
#14186=CARTESIAN_POINT('Ctrl Pts',(-16.4425188328326,8.6595836864797,5.55489475436157));
#14187=CARTESIAN_POINT('Ctrl Pts',(-16.908486954743,10.4850299113492,5.44375360683254));
#14188=CARTESIAN_POINT('Ctrl Pts',(-15.6275015719515,11.8664989271813,5.33261245930353));
#14189=CARTESIAN_POINT('Ctrl Pts',(-13.7721260589331,11.5394486208087,5.2214713117745));
#14190=CARTESIAN_POINT('Ctrl Pts',(-13.0406978065988,9.80324790916912,5.11033016424548));
#14191=CARTESIAN_POINT('Ctrl Pts',(-14.1027373194897,8.24714628330515,4.99918901671647));
#14192=CARTESIAN_POINT('Ctrl Pts',(-15.9860956161181,8.2955376489092,4.88804786918745));
#14193=CARTESIAN_POINT('Ctrl Pts',(-16.9668209718389,9.90412646355499,4.77690672165843));
#14194=CARTESIAN_POINT('Ctrl Pts',(-16.1471961698029,11.6004741229444,4.66576557412941));
#14195=CARTESIAN_POINT('Ctrl Pts',(-14.2774733492598,11.8318110462748,4.55462442660038));
#14196=CARTESIAN_POINT('Ctrl Pts',(-13.0691228591274,10.3863805599598,4.44348327907137));
#14197=CARTESIAN_POINT('Ctrl Pts',(-13.6282209649552,8.58727258493754,4.33234213154234));
#14198=CARTESIAN_POINT('Ctrl Pts',(-15.442991365066,8.0813194323332,4.22120098401333));
#14199=CARTESIAN_POINT('Ctrl Pts',(-16.8522649836184,9.3316506147811,4.11005983648431));
#14200=CARTESIAN_POINT('Ctrl Pts',(-16.5660484669655,11.1937624007216,3.99891868895529));
#14201=CARTESIAN_POINT('Ctrl Pts',(-14.846333098649,11.9631512814075,3.88777754142627));
#14202=CARTESIAN_POINT('Ctrl Pts',(-13.2672783364837,10.9355490938709,3.77663639389725));
#14203=CARTESIAN_POINT('Ctrl Pts',(-13.2742884805443,9.05158225349828,3.66549524636823));
#14204=CARTESIAN_POINT('Ctrl Pts',(-14.8609467221099,8.03575952180664,3.5543540988392));
#14205=CARTESIAN_POINT('Ctrl Pts',(-16.5748888366715,8.8179248660152,3.44321295131019));
#14206=CARTESIAN_POINT('Ctrl Pts',(-16.8472399746527,10.6821150535684,3.33207180378116));
#14207=CARTESIAN_POINT('Ctrl Pts',(-15.4287006719665,11.921924089068,3.22093065625215));
#14208=CARTESIAN_POINT('Ctrl Pts',(-13.6177457231939,11.4024797982418,3.10978950872313));
#14209=CARTESIAN_POINT('Ctrl Pts',(-13.0720516908598,9.59926094832275,2.99864836119411));
#14210=CARTESIAN_POINT('Ctrl Pts',(-14.2911253177228,8.16286278268615,2.88750721366509));
#14211=CARTESIAN_POINT('Ctrl Pts',(-16.1590748027858,8.40810739322197,2.77636606613607));
#14212=CARTESIAN_POINT('Ctrl Pts',(-16.9660530383818,10.1105075589387,2.66522491860705));
#14213=CARTESIAN_POINT('Ctrl Pts',(-15.9733840520667,11.7117534747863,2.55408377107803));
#14214=CARTESIAN_POINT('Ctrl Pts',(-14.08971778817,11.7461279342581,2.44294262354901));
#14215=CARTESIAN_POINT('Ctrl Pts',(-13.039287871942,10.1821659194628,2.33180147601999));
#14216=CARTESIAN_POINT('Ctrl Pts',(-13.7836163199646,8.45145641986686,2.22066032849097));
#14217=CARTESIAN_POINT('Ctrl Pts',(-15.6413742968694,8.13822249874073,2.10951918096195));
#14218=CARTESIAN_POINT('Ctrl Pts',(-16.9120436018175,9.52918607960339,1.99837803343293));
#14219=CARTESIAN_POINT('Ctrl Pts',(-16.4325037837013,11.351114139767,1.88723688590391));
#14220=CARTESIAN_POINT('Ctrl Pts',(-14.6417066452378,11.9362856745195,1.77609573837489));
#14221=CARTESIAN_POINT('Ctrl Pts',(-13.1788770626978,10.7490579702873,1.66495459084587));
#14222=CARTESIAN_POINT('Ctrl Pts',(-13.3830314476372,8.87617199210746,1.55381344331685));
#14223=CARTESIAN_POINT('Ctrl Pts',(-15.0672948586319,8.03199417220646,1.44267229578783));
#14224=CARTESIAN_POINT('Ctrl Pts',(-16.6899593301811,8.98925024452329,1.33153114825881));
#14225=CARTESIAN_POINT('Ctrl Pts',(-16.7657016246685,10.8717083019789,1.22039000072979));
#14226=CARTESIAN_POINT('Ctrl Pts',(-15.22519088697,11.9562359044779,1.10924885320077));
#14227=CARTESIAN_POINT('Ctrl Pts',(-13.4785484877468,11.2501085845661,0.998107705671749));
#14228=CARTESIAN_POINT('Ctrl Pts',(-13.1245842530937,9.39966950168421,0.886966558142732));
#14229=CARTESIAN_POINT('Ctrl Pts',(-14.4872983423832,8.09877206801491,0.77582541061371));
#14230=CARTESIAN_POINT('Ctrl Pts',(-16.3193252756259,8.53813924368035,0.664684263084692));
#14231=CARTESIAN_POINT('Ctrl Pts',(-16.9436823523983,10.315721757665,0.553543115555671));
#14232=CARTESIAN_POINT('Ctrl Pts',(-15.7888920442232,11.8041387854927,0.442401968026653));
#14233=CARTESIAN_POINT('Ctrl Pts',(-13.9119373633139,11.6414407384693,0.331260820497631));
#14234=CARTESIAN_POINT('Ctrl Pts',(-13.0310370233095,9.97560805685666,0.220119672968611));
#14235=CARTESIAN_POINT('Ctrl Pts',(-13.9522834796021,8.33331535535093,0.108978525439592));
#14236=CARTESIAN_POINT('Ctrl Pts',(-15.8328831148959,8.21427038628653,-0.00216262208942864));
#14237=CARTESIAN_POINT('Ctrl Pts',(-16.9505144549114,9.73459839514212,-0.113303769618448));
#14238=CARTESIAN_POINT('Ctrl Pts',(-16.5058833578897,10.9026562341787,-0.187397867971127));
#14239=CARTESIAN_POINT('Ctrl Pts',(-16.0856682637067,11.2636773406135,-0.224444917147467));
#14240=CARTESIAN_POINT('Ctrl Pts',(-13.6322193753412,11.1633123698098,8.07481497238249));
#14241=CARTESIAN_POINT('Ctrl Pts',(-13.2453789997699,10.7084794424949,8.03776792320615));
#14242=CARTESIAN_POINT('Ctrl Pts',(-12.9678844669477,9.3903368508222,7.96367382485348));
#14243=CARTESIAN_POINT('Ctrl Pts',(-14.412735155875,7.95914047883512,7.85253267732443));
#14244=CARTESIAN_POINT('Ctrl Pts',(-16.3949596563776,8.40125966486316,7.74139152979544));
#14245=CARTESIAN_POINT('Ctrl Pts',(-17.1003553460767,10.3042270419099,7.6302503822664));
#14246=CARTESIAN_POINT('Ctrl Pts',(-15.8831401201015,11.9300354837897,7.51910923473739));
#14247=CARTESIAN_POINT('Ctrl Pts',(-13.8575477979503,11.7884864584586,7.40796808720837));
#14248=CARTESIAN_POINT('Ctrl Pts',(-12.8777036295836,10.0101780566413,7.29682693967935));
#14249=CARTESIAN_POINT('Ctrl Pts',(-13.8405294795313,8.22237225325032,7.18568579215033));
#14250=CARTESIAN_POINT('Ctrl Pts',(-15.864686828581,8.0618299096558,7.07454464462131));
#14251=CARTESIAN_POINT('Ctrl Pts',(-17.0973450598001,9.67536369518652,6.96340349709229));
#14252=CARTESIAN_POINT('Ctrl Pts',(-16.4101760177214,11.5860815627155,6.85226234956327));
#14253=CARTESIAN_POINT('Ctrl Pts',(-14.4321878727924,12.0449502551816,6.74112120203426));
#14254=CARTESIAN_POINT('Ctrl Pts',(-12.973952360191,10.6319589479372,6.62998005450522));
#14255=CARTESIAN_POINT('Ctrl Pts',(-13.3702808278786,8.64049399125046,6.51883890697622));
#14256=CARTESIAN_POINT('Ctrl Pts',(-15.2583897561767,7.89346884722859,6.40769775944719));
#14257=CARTESIAN_POINT('Ctrl Pts',(-16.9099789365563,9.07467812810877,6.29655661191818));
#14258=CARTESIAN_POINT('Ctrl Pts',(-16.8132489010525,11.1028909361887,6.18541546438915));
#14259=CARTESIAN_POINT('Ctrl Pts',(-15.056742514914,12.1215607429465,6.07427431686013));
#14260=CARTESIAN_POINT('Ctrl Pts',(-13.2482962713414,11.1982378481243,5.96313316933111));
#14261=CARTESIAN_POINT('Ctrl Pts',(-13.0432903673187,9.17809533599028,5.85199202180209));
#14262=CARTESIAN_POINT('Ctrl Pts',(-14.6293791002458,7.91029189187743,5.74085087427308));
#14263=CARTESIAN_POINT('Ctrl Pts',(-16.5547195523731,8.55532461447468,5.62970972674405));
#14264=CARTESIAN_POINT('Ctrl Pts',(-17.0569311931696,10.5227560774231,5.51856857921503));
#14265=CARTESIAN_POINT('Ctrl Pts',(-15.6763093422789,12.0116772901148,5.40742743168601));
#14266=CARTESIAN_POINT('Ctrl Pts',(-13.6766206578547,11.6591886470871,5.296286284157));
#14267=CARTESIAN_POINT('Ctrl Pts',(-12.8883011023801,9.78794431266843,5.18514513662797));
#14268=CARTESIAN_POINT('Ctrl Pts',(-14.0329472300443,8.11080737126729,5.07400398909896));
#14269=CARTESIAN_POINT('Ctrl Pts',(-16.0627952301169,8.16296267112078,4.96286284156994));
#14270=CARTESIAN_POINT('Ctrl Pts',(-17.1198024950087,9.89666931323625,4.85172169404091));
#14271=CARTESIAN_POINT('Ctrl Pts',(-16.2364263640828,11.7249607806665,4.7405805465119));
#14272=CARTESIAN_POINT('Ctrl Pts',(-14.2212744225941,11.9742913472431,4.62943939898287));
#14273=CARTESIAN_POINT('Ctrl Pts',(-12.9189370871157,10.4164336697406,4.51829825145386));
#14274=CARTESIAN_POINT('Ctrl Pts',(-13.5215224655807,8.47738907501246,4.40715710392483));
#14275=CARTESIAN_POINT('Ctrl Pts',(-15.4774477262444,7.9320823233535,4.29601595639582));
#14276=CARTESIAN_POINT('Ctrl Pts',(-16.9963362145871,9.27966565609687,4.18487480886679));
#14277=CARTESIAN_POINT('Ctrl Pts',(-16.6878574588688,11.2866145682447,4.07373366133778));
#14278=CARTESIAN_POINT('Ctrl Pts',(-14.8343807161159,12.1158473719732,3.96259251380876));
#14279=CARTESIAN_POINT('Ctrl Pts',(-13.1325053179379,11.0083171431391,3.85145136627974));
#14280=CARTESIAN_POINT('Ctrl Pts',(-13.140060718802,8.97781326611282,3.74031021875072));
#14281=CARTESIAN_POINT('Ctrl Pts',(-14.8501310034664,7.8829787123033,3.6291690712217));
#14282=CARTESIAN_POINT('Ctrl Pts',(-16.697385442365,8.72598174710033,3.51802792369268));
#14283=CARTESIAN_POINT('Ctrl Pts',(-16.990920354834,10.7351707212503,3.40688677616366));
#14284=CARTESIAN_POINT('Ctrl Pts',(-15.4620454871379,12.0714134827505,3.29574562863464));
#14285=CARTESIAN_POINT('Ctrl Pts',(-13.5102324478621,11.5115662371307,3.18460448110562));
#14286=CARTESIAN_POINT('Ctrl Pts',(-12.9220937266384,9.56809101908315,3.0734633335766));
#14287=CARTESIAN_POINT('Ctrl Pts',(-14.2359882563512,8.0199682062094,2.96232218604758));
#14288=CARTESIAN_POINT('Ctrl Pts',(-16.2492289303534,8.28428821537383,2.85118103851856));
#14289=CARTESIAN_POINT('Ctrl Pts',(-17.118974830833,10.1191029598066,2.74003989098954));
#14290=CARTESIAN_POINT('Ctrl Pts',(-16.0490949464727,11.8448955642867,2.62889874346052));
#14291=CARTESIAN_POINT('Ctrl Pts',(-14.018915025095,11.881943707456,2.5177575959315));
#14292=CARTESIAN_POINT('Ctrl Pts',(-12.8867815014373,10.1963349873281,2.40661644840248));
#14293=CARTESIAN_POINT('Ctrl Pts',(-13.6890046441715,8.33100897753458,2.29547530087345));
#14294=CARTESIAN_POINT('Ctrl Pts',(-15.6912611031735,7.99341137356774,2.18433415334444));
#14295=CARTESIAN_POINT('Ctrl Pts',(-17.0607644802102,9.49256564912037,2.07319300581542));
#14296=CARTESIAN_POINT('Ctrl Pts',(-16.5439255215792,11.4562053005982,1.9620518582864));
#14297=CARTESIAN_POINT('Ctrl Pts',(-14.6138381895228,12.0868921282949,1.85091071075738));
#14298=CARTESIAN_POINT('Ctrl Pts',(-13.0372280947354,10.807320532502,1.73976956322836));
#14299=CARTESIAN_POINT('Ctrl Pts',(-13.2572618348459,8.78875939945676,1.62862841569934));
#14300=CARTESIAN_POINT('Ctrl Pts',(-15.0725291275981,7.87892048962247,1.51748726817032));
#14301=CARTESIAN_POINT('Ctrl Pts',(-16.8214062468694,8.91063300413882,1.4063461206413));
#14302=CARTESIAN_POINT('Ctrl Pts',(-16.9030398612811,10.9395107434343,1.29520497311228));
#14303=CARTESIAN_POINT('Ctrl Pts',(-15.242706484671,12.1083941093329,1.18406382558326));
#14304=CARTESIAN_POINT('Ctrl Pts',(-13.3602082965927,11.3473434209507,1.07292267805424));
#14305=CARTESIAN_POINT('Ctrl Pts',(-12.9787123300025,9.35297512769056,0.961781530525221));
#14306=CARTESIAN_POINT('Ctrl Pts',(-14.4474198371014,7.95089244445364,0.8506403829962));
#14307=CARTESIAN_POINT('Ctrl Pts',(-16.4219438632409,8.42443408781415,0.739499235467181));
#14308=CARTESIAN_POINT('Ctrl Pts',(-17.0948641280075,10.3402789471993,0.628358087938161));
#14309=CARTESIAN_POINT('Ctrl Pts',(-15.8502529450219,11.9444667072335,0.517216940409141));
#14310=CARTESIAN_POINT('Ctrl Pts',(-13.8273066410226,11.7691138251199,0.40607579288012));
#14311=CARTESIAN_POINT('Ctrl Pts',(-12.8778888926195,9.97371082438428,0.294934645351101));
#14312=CARTESIAN_POINT('Ctrl Pts',(-13.8707909231185,8.20367876959515,0.183793497822081));
#14313=CARTESIAN_POINT('Ctrl Pts',(-15.8976656901092,8.07537435040597,0.0726523502930605));
#14314=CARTESIAN_POINT('Ctrl Pts',(-17.1022276390544,9.71395516307158,-0.0384887972359591));
#14315=CARTESIAN_POINT('Ctrl Pts',(-16.6230126406787,10.9728658402285,-0.112582895588638));
#14316=CARTESIAN_POINT('Ctrl Pts',(-16.170112749004,11.361967569938,-0.149629944764978));
#14317=CARTESIAN_POINT('Ctrl Pts',(-13.5335096305347,11.247266086571,8.14962994476498));
#14318=CARTESIAN_POINT('Ctrl Pts',(-13.1187518286854,10.7596088587978,8.11258289558864));
#14319=CARTESIAN_POINT('Ctrl Pts',(-12.8212311205934,9.34633879090798,8.03848879723596));
#14320=CARTESIAN_POINT('Ctrl Pts',(-14.3703535327899,7.81185609792774,7.92734764970693));
#14321=CARTESIAN_POINT('Ctrl Pts',(-16.4956308526308,8.28588206143169,7.81620650217792));
#14322=CARTESIAN_POINT('Ctrl Pts',(-17.2519334109186,10.3261824440619,7.7050653546489));
#14323=CARTESIAN_POINT('Ctrl Pts',(-15.9468744166049,12.0693219356063,7.59392420711988));
#14324=CARTESIAN_POINT('Ctrl Pts',(-13.7750995140042,11.9175576258092,7.48278305959087));
#14325=CARTESIAN_POINT('Ctrl Pts',(-12.7245421288643,10.0109125847927,7.37164191206184));
#14326=CARTESIAN_POINT('Ctrl Pts',(-13.7568530206586,8.09408473544294,7.26050076453282));
#14327=CARTESIAN_POINT('Ctrl Pts',(-15.9270893912785,7.92195640102419,7.1493596170038));
#14328=CARTESIAN_POINT('Ctrl Pts',(-17.2487058788463,9.65193540103954,7.03821846947478));
#14329=CARTESIAN_POINT('Ctrl Pts',(-16.5119453455887,11.7005456101477,6.92707732194576));
#14330=CARTESIAN_POINT('Ctrl Pts',(-14.3912101098645,12.1925298554418,6.81593617441674));
#14331=CARTESIAN_POINT('Ctrl Pts',(-12.8277369204591,10.6775660470248,6.70479502688772));
#14332=CARTESIAN_POINT('Ctrl Pts',(-13.252667549341,8.54238140742879,6.59365387935871));
#14333=CARTESIAN_POINT('Ctrl Pts',(-15.27703718138,7.74144508788578,6.48251273182967));
#14334=CARTESIAN_POINT('Ctrl Pts',(-17.0478179510987,9.0078996665693,6.37137158430067));
#14335=CARTESIAN_POINT('Ctrl Pts',(-16.9441071198828,11.1824841698534,6.26023043677164));
#14336=CARTESIAN_POINT('Ctrl Pts',(-15.0608374984705,12.2746691550355,6.14908928924262));
#14337=CARTESIAN_POINT('Ctrl Pts',(-13.1218796333842,11.2847120604895,6.03794814171361));
#14338=CARTESIAN_POINT('Ctrl Pts',(-12.9020789003479,9.11878026880993,5.92680699418458));
#14339=CARTESIAN_POINT('Ctrl Pts',(-14.6026321981658,7.759482214979,5.81566584665557));
#14340=CARTESIAN_POINT('Ctrl Pts',(-16.6669202719137,8.45106554246967,5.70452469912654));
#14341=CARTESIAN_POINT('Ctrl Pts',(-17.2053754315962,10.5604822434969,5.59338355159752));
#14342=CARTESIAN_POINT('Ctrl Pts',(-15.7251171126062,12.1568556530484,5.4822424040685));
#14343=CARTESIAN_POINT('Ctrl Pts',(-13.5811152567764,11.7789286733654,5.37110125653948));
#14344=CARTESIAN_POINT('Ctrl Pts',(-12.7359043981615,9.77264071616773,5.25996010901047));
#14345=CARTESIAN_POINT('Ctrl Pts',(-13.9631571405989,7.97446845922946,5.14881896148145));
#14346=CARTESIAN_POINT('Ctrl Pts',(-16.1394948441157,8.03038769333235,5.03767781395242));
#14347=CARTESIAN_POINT('Ctrl Pts',(-17.2727840181784,9.88921216291753,4.9265366664234));
#14348=CARTESIAN_POINT('Ctrl Pts',(-16.3256565583627,11.8494474383885,4.81539551889438));
#14349=CARTESIAN_POINT('Ctrl Pts',(-14.1650754959284,12.1167716482113,4.70425437136536));
#14350=CARTESIAN_POINT('Ctrl Pts',(-12.7687513151041,10.4464867795214,4.59311322383634));
#14351=CARTESIAN_POINT('Ctrl Pts',(-13.4148239662062,8.36750556508739,4.48197207630732));
#14352=CARTESIAN_POINT('Ctrl Pts',(-15.5119040874227,7.78284521437382,4.3708309287783));
#14353=CARTESIAN_POINT('Ctrl Pts',(-17.1404074455559,9.22768069741262,4.25968978124929));
#14354=CARTESIAN_POINT('Ctrl Pts',(-16.8096664507721,11.3794667357678,4.14854863372026));
#14355=CARTESIAN_POINT('Ctrl Pts',(-14.8224283335829,12.2685434625389,4.03740748619125));
#14356=CARTESIAN_POINT('Ctrl Pts',(-12.9977322993921,11.0810851924073,3.92626633866222));
#14357=CARTESIAN_POINT('Ctrl Pts',(-13.0058329570596,8.90404427872736,3.81512519113321));
#14358=CARTESIAN_POINT('Ctrl Pts',(-14.839315284823,7.73019790279997,3.70398404360418));
#14359=CARTESIAN_POINT('Ctrl Pts',(-16.8198820480584,8.63403862818544,3.59284289607517));
#14360=CARTESIAN_POINT('Ctrl Pts',(-17.1346007350153,10.7882263889324,3.48170174854614));
#14361=CARTESIAN_POINT('Ctrl Pts',(-15.4953903023094,12.220902876433,3.37056060101713));
#14362=CARTESIAN_POINT('Ctrl Pts',(-13.4027191725303,11.6206526760196,3.2594194534881));
#14363=CARTESIAN_POINT('Ctrl Pts',(-12.7721357624171,9.53692108984355,3.14827830595909));
#14364=CARTESIAN_POINT('Ctrl Pts',(-14.1808511949796,7.87707362973266,3.03713715843006));
#14365=CARTESIAN_POINT('Ctrl Pts',(-16.339383057921,8.16046903752571,2.92599601090105));
#14366=CARTESIAN_POINT('Ctrl Pts',(-17.2718966232842,10.1276983606744,2.81485486337203));
#14367=CARTESIAN_POINT('Ctrl Pts',(-16.1248058408786,11.9780376537872,2.70371371584301));
#14368=CARTESIAN_POINT('Ctrl Pts',(-13.9481122620199,12.0177594806538,2.59257256831399));
#14369=CARTESIAN_POINT('Ctrl Pts',(-12.7342751309326,10.2105040551935,2.48143142078497));
#14370=CARTESIAN_POINT('Ctrl Pts',(-13.5943929683785,8.21056153520229,2.37029027325595));
#14371=CARTESIAN_POINT('Ctrl Pts',(-15.7411479094776,7.84860024839477,2.25914912572693));
#14372=CARTESIAN_POINT('Ctrl Pts',(-17.2094853586029,9.45594521863734,2.14800797819791));
#14373=CARTESIAN_POINT('Ctrl Pts',(-16.6553472594571,11.5612964614294,2.03686683066889));
#14374=CARTESIAN_POINT('Ctrl Pts',(-14.5859697338077,12.2374985820703,1.92572568313987));
#14375=CARTESIAN_POINT('Ctrl Pts',(-12.895579126773,10.8655830947167,1.81458453561085));
#14376=CARTESIAN_POINT('Ctrl Pts',(-13.1314922220546,8.70134680680606,1.70344338808183));
#14377=CARTESIAN_POINT('Ctrl Pts',(-15.0777633965643,7.72584680703849,1.59230224055281));
#14378=CARTESIAN_POINT('Ctrl Pts',(-16.9528531635576,8.83201576375435,1.48116109302379));
#14379=CARTESIAN_POINT('Ctrl Pts',(-17.0403780978937,11.0073131848898,1.37001994549477));
#14380=CARTESIAN_POINT('Ctrl Pts',(-15.260222082372,12.260552314188,1.25887879796575));
#14381=CARTESIAN_POINT('Ctrl Pts',(-13.2418681054385,11.4445782573353,1.14773765043673));
#14382=CARTESIAN_POINT('Ctrl Pts',(-12.8328404069114,9.30628075369691,1.03659650290771));
#14383=CARTESIAN_POINT('Ctrl Pts',(-14.4075413318195,7.80301282089239,0.925455355378688));
#14384=CARTESIAN_POINT('Ctrl Pts',(-16.5245624508558,8.31072893194794,0.814314207849671));
#14385=CARTESIAN_POINT('Ctrl Pts',(-17.2460459036167,10.3648361367336,0.703173060320649));
#14386=CARTESIAN_POINT('Ctrl Pts',(-15.9116138458206,12.0847946289742,0.592031912791631));
#14387=CARTESIAN_POINT('Ctrl Pts',(-13.7426759187313,11.8967869117706,0.480890765262609));
#14388=CARTESIAN_POINT('Ctrl Pts',(-12.7247407619296,9.97181359191189,0.369749617733589));
#14389=CARTESIAN_POINT('Ctrl Pts',(-13.789298366635,8.07404218383939,0.25860847020457));
#14390=CARTESIAN_POINT('Ctrl Pts',(-15.9624482653224,7.93647831452539,0.147467322675549));
#14391=CARTESIAN_POINT('Ctrl Pts',(-17.2539408231974,9.69331193100106,0.03632617514653));
#14392=CARTESIAN_POINT('Ctrl Pts',(-16.7401419234678,11.0430754462783,-0.0377679232061492));
#14393=CARTESIAN_POINT('Ctrl Pts',(-16.2545572343013,11.4602577992624,-0.0748149723824891));
#14394=CARTESIAN_POINT('Ctrl Pts',(-13.4347998857283,11.3312198033322,8.22444491714747));
#14395=CARTESIAN_POINT('Ctrl Pts',(-12.9921246576009,10.8107382751008,8.18739786797113));
#14396=CARTESIAN_POINT('Ctrl Pts',(-12.6745777742391,9.30234073099377,8.11330376961845));
#14397=CARTESIAN_POINT('Ctrl Pts',(-14.3279719097048,7.66457171702036,8.00216262208942));
#14398=CARTESIAN_POINT('Ctrl Pts',(-16.596302048884,8.17050445800021,7.89102147456042));
#14399=CARTESIAN_POINT('Ctrl Pts',(-17.4035114757606,10.3481378462139,7.77988032703138));
#14400=CARTESIAN_POINT('Ctrl Pts',(-16.0106087131083,12.2086083874229,7.66873917950237));
#14401=CARTESIAN_POINT('Ctrl Pts',(-13.6926512300581,12.0466287931598,7.55759803197335));
#14402=CARTESIAN_POINT('Ctrl Pts',(-12.5713806281451,10.011647112944,7.44645688444433));
#14403=CARTESIAN_POINT('Ctrl Pts',(-13.673176561786,7.96579721763555,7.33531573691531));
#14404=CARTESIAN_POINT('Ctrl Pts',(-15.989491953976,7.78208289239259,7.22417458938629));
#14405=CARTESIAN_POINT('Ctrl Pts',(-17.4000666978926,9.62850710689255,7.11303344185727));
#14406=CARTESIAN_POINT('Ctrl Pts',(-16.613714673456,11.81500965758,7.00189229432825));
#14407=CARTESIAN_POINT('Ctrl Pts',(-14.3502323469365,12.3401094557021,6.89075114679924));
#14408=CARTESIAN_POINT('Ctrl Pts',(-12.6815214807272,10.7231731461125,6.77960999927021));
#14409=CARTESIAN_POINT('Ctrl Pts',(-13.1350542708035,8.44426882360712,6.66846885174119));
#14410=CARTESIAN_POINT('Ctrl Pts',(-15.2956846065833,7.58942132854296,6.55732770421217));
#14411=CARTESIAN_POINT('Ctrl Pts',(-17.1856569656411,8.94112120502986,6.44618655668315));
#14412=CARTESIAN_POINT('Ctrl Pts',(-17.0749653387131,11.262077403518,6.33504540915413));
#14413=CARTESIAN_POINT('Ctrl Pts',(-15.0649324820269,12.4277775671245,6.22390426162511));
#14414=CARTESIAN_POINT('Ctrl Pts',(-12.9954629954269,11.3711862728547,6.11276311409609));
#14415=CARTESIAN_POINT('Ctrl Pts',(-12.7608674333771,9.05946520162959,6.00162196656707));
#14416=CARTESIAN_POINT('Ctrl Pts',(-14.5758852960858,7.60867253808055,5.89048081903805));
#14417=CARTESIAN_POINT('Ctrl Pts',(-16.7791209914542,8.34680647046468,5.77933967150903));
#14418=CARTESIAN_POINT('Ctrl Pts',(-17.3538196700229,10.5982084095707,5.66819852398001));
#14419=CARTESIAN_POINT('Ctrl Pts',(-15.7739248829336,12.3020340159819,5.557057376451));
#14420=CARTESIAN_POINT('Ctrl Pts',(-13.485609855698,11.8986686996438,5.44591622892196));
#14421=CARTESIAN_POINT('Ctrl Pts',(-12.5835076939429,9.75733711966703,5.33477508139296));
#14422=CARTESIAN_POINT('Ctrl Pts',(-13.8933670511534,7.83812954719161,5.22363393386392));
#14423=CARTESIAN_POINT('Ctrl Pts',(-16.2161944581144,7.89781271554394,5.11249278633492));
#14424=CARTESIAN_POINT('Ctrl Pts',(-17.4257655413481,9.88175501259879,5.00135163880589));
#14425=CARTESIAN_POINT('Ctrl Pts',(-16.4148867526426,11.9739340961105,4.89021049127687));
#14426=CARTESIAN_POINT('Ctrl Pts',(-14.1088765692626,12.2592519491796,4.77906934374786));
#14427=CARTESIAN_POINT('Ctrl Pts',(-12.6185655430924,10.4765398893022,4.66792819621883));
#14428=CARTESIAN_POINT('Ctrl Pts',(-13.3081254668317,8.25762205516231,4.55678704868981));
#14429=CARTESIAN_POINT('Ctrl Pts',(-15.5463604486011,7.63360810539413,4.44564590116079));
#14430=CARTESIAN_POINT('Ctrl Pts',(-17.2844786765246,9.17569573872837,4.33450475363177));
#14431=CARTESIAN_POINT('Ctrl Pts',(-16.9314754426754,11.4723189032909,4.22336360610276));
#14432=CARTESIAN_POINT('Ctrl Pts',(-14.8104759510498,12.4212395531045,4.11222245857373));
#14433=CARTESIAN_POINT('Ctrl Pts',(-12.8629592808463,11.1538532416754,4.00108131104471));
#14434=CARTESIAN_POINT('Ctrl Pts',(-12.8716051953172,8.83027529134189,3.8899401635157));
#14435=CARTESIAN_POINT('Ctrl Pts',(-14.8284995661796,7.57741709329663,3.77879901598667));
#14436=CARTESIAN_POINT('Ctrl Pts',(-16.9423786537519,8.54209550927056,3.66765786845766));
#14437=CARTESIAN_POINT('Ctrl Pts',(-17.2782811151966,10.8412820566144,3.55651672092863));
#14438=CARTESIAN_POINT('Ctrl Pts',(-15.5287351174808,12.3703922701155,3.44537557339962));
#14439=CARTESIAN_POINT('Ctrl Pts',(-13.2952058971985,11.7297391149084,3.33423442587059));
#14440=CARTESIAN_POINT('Ctrl Pts',(-12.6221777981957,9.50575116060393,3.22309327834158));
#14441=CARTESIAN_POINT('Ctrl Pts',(-14.125714133608,7.73417905325592,3.11195213081255));
#14442=CARTESIAN_POINT('Ctrl Pts',(-16.4295371854886,8.03664985967757,3.00081098328354));
#14443=CARTESIAN_POINT('Ctrl Pts',(-17.4248184157354,10.1362937615422,2.88966983575451));
#14444=CARTESIAN_POINT('Ctrl Pts',(-16.2005167352846,12.1111797432876,2.7785286882255));
#14445=CARTESIAN_POINT('Ctrl Pts',(-13.8773094989449,12.1535752538516,2.66738754069648));
#14446=CARTESIAN_POINT('Ctrl Pts',(-12.5817687604279,10.2246731230589,2.55624639316746));
#14447=CARTESIAN_POINT('Ctrl Pts',(-13.4997812925854,8.09011409287,2.44510524563844));
#14448=CARTESIAN_POINT('Ctrl Pts',(-15.7910347157817,7.70378912322181,2.33396409810942));
#14449=CARTESIAN_POINT('Ctrl Pts',(-17.3582062369956,9.4193247881543,2.2228229505804));
#14450=CARTESIAN_POINT('Ctrl Pts',(-16.766768997335,11.6663876222607,2.11168180305137));
#14451=CARTESIAN_POINT('Ctrl Pts',(-14.5581012780927,12.3881050358458,2.00054065552236));
#14452=CARTESIAN_POINT('Ctrl Pts',(-12.7539301588106,10.9238456569314,1.88939950799334));
#14453=CARTESIAN_POINT('Ctrl Pts',(-13.0057226092633,8.61393421415536,1.77825836046432));
#14454=CARTESIAN_POINT('Ctrl Pts',(-15.0829976655305,7.57277312445451,1.6671172129353));
#14455=CARTESIAN_POINT('Ctrl Pts',(-17.0843000802458,8.75339852336988,1.55597606540628));
#14456=CARTESIAN_POINT('Ctrl Pts',(-17.1777163345064,11.0751156263452,1.44483491787726));
#14457=CARTESIAN_POINT('Ctrl Pts',(-15.277737680073,12.4127105190431,1.33369377034824));
#14458=CARTESIAN_POINT('Ctrl Pts',(-13.1235279142844,11.5418130937198,1.22255262281922));
#14459=CARTESIAN_POINT('Ctrl Pts',(-12.6869684838201,9.25958637970326,1.1114114752902));
#14460=CARTESIAN_POINT('Ctrl Pts',(-14.3676628265377,7.65513319733112,1.00027032776118));
#14461=CARTESIAN_POINT('Ctrl Pts',(-16.6271810384708,8.19702377608174,0.88912918023216));
#14462=CARTESIAN_POINT('Ctrl Pts',(-17.3972276792259,10.3893933262678,0.777988032703138));
#14463=CARTESIAN_POINT('Ctrl Pts',(-15.9729747466193,12.225122550715,0.66684688517412));
#14464=CARTESIAN_POINT('Ctrl Pts',(-13.6580451964401,12.0244599984212,0.555705737645099));
#14465=CARTESIAN_POINT('Ctrl Pts',(-12.5715926312396,9.9699163594395,0.444564590116078));
#14466=CARTESIAN_POINT('Ctrl Pts',(-13.7078058101514,7.94440559808363,0.333423442587059));
#14467=CARTESIAN_POINT('Ctrl Pts',(-16.0272308405357,7.79758227864481,0.222282295058039));
#14468=CARTESIAN_POINT('Ctrl Pts',(-17.4056540073404,9.67266869893052,0.111141147529019));
#14469=CARTESIAN_POINT('Ctrl Pts',(-16.8572712062568,11.1132850523281,0.0370470491763399));
#14470=CARTESIAN_POINT('Ctrl Pts',(-16.3390017195986,11.5585480285869,0.));
#14471=CARTESIAN_POINT('Ctrl Pts',(-13.7309291201476,11.0793586530485,8.));
#14472=CARTESIAN_POINT('Ctrl Pts',(-13.6852152716991,11.0367124842021,8.));
#14473=CARTESIAN_POINT('Ctrl Pts',(-13.6422346164434,10.9914156431349,8.));
#14474=CARTESIAN_POINT('Ctrl Pts',(-13.601998738308,10.9438052169207,8.));
#14475=CARTESIAN_POINT('Ctrl Pts',(-13.5764667336105,10.9135936325813,8.));
#14476=CARTESIAN_POINT('Ctrl Pts',(-13.5520403842569,10.8824494351603,8.));
#14477=CARTESIAN_POINT('Ctrl Pts',(-13.5287280007931,10.850449719119,8.));
#14478=CARTESIAN_POINT('Ctrl Pts',(-13.5126489582125,10.8283788400261,8.));
#14479=CARTESIAN_POINT('Ctrl Pts',(-13.497099934263,10.8059008351366,8.));
#14480=CARTESIAN_POINT('Ctrl Pts',(-13.4820849794618,10.7830393699546,8.));
#14481=CARTESIAN_POINT('Ctrl Pts',(-13.4742666591409,10.7711353542471,8.));
#14482=CARTESIAN_POINT('Ctrl Pts',(-13.4665935957101,10.7591278087324,8.));
#14483=CARTESIAN_POINT('Ctrl Pts',(-13.4590733535016,10.7470317213655,8.));
#14484=CARTESIAN_POINT('Ctrl Pts',(-13.4242375073996,10.6909992923205,8.));
#14485=CARTESIAN_POINT('Ctrl Pts',(-13.3926366847534,10.6330080071976,8.));
#14486=CARTESIAN_POINT('Ctrl Pts',(-13.3643038144212,10.5734090455691,8.));
#14487=CARTESIAN_POINT('Ctrl Pts',(-13.3438796821625,10.5304463291022,8.));
#14488=CARTESIAN_POINT('Ctrl Pts',(-13.3251543285811,10.4866471329582,8.));
#14489=CARTESIAN_POINT('Ctrl Pts',(-13.3081517237824,10.4421310384001,8.));
#14490=CARTESIAN_POINT('Ctrl Pts',(-13.3034050847435,10.4297034230557,8.));
#14491=CARTESIAN_POINT('Ctrl Pts',(-13.2987927744426,10.4172198853085,8.));
#14492=CARTESIAN_POINT('Ctrl Pts',(-13.2943154661998,10.4046829194981,8.));
#14493=CARTESIAN_POINT('Ctrl Pts',(-13.2899383781238,10.3924265814078,8.));
#14494=CARTESIAN_POINT('Ctrl Pts',(-13.2856933225078,10.3801275302436,8.));
#14495=CARTESIAN_POINT('Ctrl Pts',(-13.2815814261066,10.367791367639,8.));
#14496=CARTESIAN_POINT('Ctrl Pts',(-13.2601244711192,10.303418032346,8.));
#14497=CARTESIAN_POINT('Ctrl Pts',(-13.2422813001474,10.2380113738685,8.));
#14498=CARTESIAN_POINT('Ctrl Pts',(-13.2280844604704,10.1719275884727,8.));
#14499=CARTESIAN_POINT('Ctrl Pts',(-13.213683957365,10.1048957857298,8.));
#14500=CARTESIAN_POINT('Ctrl Pts',(-13.2030346042218,10.0371663785979,8.));
#14501=CARTESIAN_POINT('Ctrl Pts',(-13.1962126701045,9.96907944108561,8.));
#14502=CARTESIAN_POINT('Ctrl Pts',(-13.1919872272218,9.92690702186065,8.));
#14503=CARTESIAN_POINT('Ctrl Pts',(-13.1892310184523,9.88459686452187,8.));
#14504=CARTESIAN_POINT('Ctrl Pts',(-13.1879715509946,9.84222623000023,8.));
#14505=CARTESIAN_POINT('Ctrl Pts',(-13.1869384830453,9.8074720612857,8.));
#14506=CARTESIAN_POINT('Ctrl Pts',(-13.1869125402926,9.77267713446997,8.));
#14507=CARTESIAN_POINT('Ctrl Pts',(-13.1879128834702,9.73788353314392,8.));
#14508=CARTESIAN_POINT('Ctrl Pts',(-13.1883195913401,9.72373755624667,8.));
#14509=CARTESIAN_POINT('Ctrl Pts',(-13.1888962462514,9.70958938159508,8.));
#14510=CARTESIAN_POINT('Ctrl Pts',(-13.1896426561975,9.69546565230446,8.));
#14511=CARTESIAN_POINT('Ctrl Pts',(-13.1933622318364,9.62508304329351,8.));
#14512=CARTESIAN_POINT('Ctrl Pts',(-13.2012954945328,9.55518382486859,8.));
#14513=CARTESIAN_POINT('Ctrl Pts',(-13.2135052750766,9.48612542924265,8.));
#14514=CARTESIAN_POINT('Ctrl Pts',(-13.2148602658297,9.47846161520753,8.));
#14515=CARTESIAN_POINT('Ctrl Pts',(-13.2162679737953,9.4708081370592,8.));
#14516=CARTESIAN_POINT('Ctrl Pts',(-13.2177285223696,9.46316547049678,8.));
#14517=CARTESIAN_POINT('Ctrl Pts',(-13.2303835600112,9.39694498681769,8.));
#14518=CARTESIAN_POINT('Ctrl Pts',(-13.2470012041599,9.33153634460149,8.));
#14519=CARTESIAN_POINT('Ctrl Pts',(-13.2673104055905,9.26714714029771,8.));
#14520=CARTESIAN_POINT('Ctrl Pts',(-13.2891624783375,9.19786634748179,8.));
#14521=CARTESIAN_POINT('Ctrl Pts',(-13.315288085799,9.12976478423422,8.));
#14522=CARTESIAN_POINT('Ctrl Pts',(-13.3454136056875,9.06310682836119,8.));
#14523=CARTESIAN_POINT('Ctrl Pts',(-13.3509659872551,9.05082121779261,8.));
#14524=CARTESIAN_POINT('Ctrl Pts',(-13.35665441154,9.03858468597769,8.));
#14525=CARTESIAN_POINT('Ctrl Pts',(-13.3624773867768,9.02639895256681,8.));
#14526=CARTESIAN_POINT('Ctrl Pts',(-13.3674119000146,9.01607250253326,8.));
#14527=CARTESIAN_POINT('Ctrl Pts',(-13.3724389146256,9.00579117530112,8.));
#14528=CARTESIAN_POINT('Ctrl Pts',(-13.3775566194876,8.99555672351709,8.));
#14529=CARTESIAN_POINT('Ctrl Pts',(-13.4093425266683,8.93199085889207,8.));
#14530=CARTESIAN_POINT('Ctrl Pts',(-13.444627394604,8.87022282259155,8.));
#14531=CARTESIAN_POINT('Ctrl Pts',(-13.4831031309424,8.81047698893777,8.));
#14532=CARTESIAN_POINT('Ctrl Pts',(-13.5223915933793,8.74946913919547,8.));
#14533=CARTESIAN_POINT('Ctrl Pts',(-13.5650075075404,8.69056895823217,8.));
#14534=CARTESIAN_POINT('Ctrl Pts',(-13.6106773499442,8.63402362180269,8.));
#14535=CARTESIAN_POINT('Ctrl Pts',(-13.6566251153189,8.57713417978688,8.));
#14536=CARTESIAN_POINT('Ctrl Pts',(-13.7056646272697,8.52262739947179,8.));
#14537=CARTESIAN_POINT('Ctrl Pts',(-13.7575649500188,8.47077690562292,8.));
#14538=CARTESIAN_POINT('Ctrl Pts',(-13.7703956403815,8.4579585338578,8.));
#14539=CARTESIAN_POINT('Ctrl Pts',(-13.7834013784189,8.44530264814056,8.));
#14540=CARTESIAN_POINT('Ctrl Pts',(-13.7965790599829,8.43281369133694,8.));
#14541=CARTESIAN_POINT('Ctrl Pts',(-13.8068736174222,8.42305717365612,8.));
#14542=CARTESIAN_POINT('Ctrl Pts',(-13.8172743724373,8.41340154458166,8.));
#14543=CARTESIAN_POINT('Ctrl Pts',(-13.8277637530731,8.40386320384444,8.));
#14544=CARTESIAN_POINT('Ctrl Pts',(-13.8835124617526,8.35316905921277,8.));
#14545=CARTESIAN_POINT('Ctrl Pts',(-13.9418585842011,8.3056917081039,8.));
#14546=CARTESIAN_POINT('Ctrl Pts',(-14.0025043610684,8.26168470116104,8.));
#14547=CARTESIAN_POINT('Ctrl Pts',(-14.0632169295863,8.21762922751878,8.));
#14548=CARTESIAN_POINT('Ctrl Pts',(-14.1262348596866,8.1770508152945,8.));
#14549=CARTESIAN_POINT('Ctrl Pts',(-14.1913041268544,8.14023030306485,8.));
#14550=CARTESIAN_POINT('Ctrl Pts',(-14.2548907910063,8.10424874607246,8.));
#14551=CARTESIAN_POINT('Ctrl Pts',(-14.3204371099339,8.07185505382328,8.));
#14552=CARTESIAN_POINT('Ctrl Pts',(-14.3877383485173,8.04334865248953,8.));
#14553=CARTESIAN_POINT('Ctrl Pts',(-14.4022444047088,8.03720440509873,8.));
#14554=CARTESIAN_POINT('Ctrl Pts',(-14.4168320883943,8.03124091428558,8.));
#14555=CARTESIAN_POINT('Ctrl Pts',(-14.431499502301,8.02546146405585,8.));
#14556=CARTESIAN_POINT('Ctrl Pts',(-14.4438537777607,8.02059346751615,8.));
#14557=CARTESIAN_POINT('Ctrl Pts',(-14.4562646196476,8.01585604250524,8.));
#14558=CARTESIAN_POINT('Ctrl Pts',(-14.4687302296836,8.0112487681312,8.));
#14559=CARTESIAN_POINT('Ctrl Pts',(-16.6673099161007,9.99870037981829,6.87148036339021));
#14560=CARTESIAN_POINT('Ctrl Pts',(-16.6680395399047,9.91361837787032,6.87718308383007));
#14561=CARTESIAN_POINT('Ctrl Pts',(-16.6620893791087,9.82863879732174,6.88288580426994));
#14562=CARTESIAN_POINT('Ctrl Pts',(-16.6491046531255,9.7447481484841,6.8885885247098));
#14563=CARTESIAN_POINT('Ctrl Pts',(-16.5647509157971,9.19976246565146,6.92563557388614));
#14564=CARTESIAN_POINT('Ctrl Pts',(-16.1835175908403,8.70073294196944,6.96268262306248));
#14565=CARTESIAN_POINT('Ctrl Pts',(-15.6798878737819,8.47604423892347,6.99972967223882));
#14566=CARTESIAN_POINT('Ctrl Pts',(-15.1762581567236,8.25135553587751,7.03677672141516));
#14567=CARTESIAN_POINT('Ctrl Pts',(-14.5502320475638,8.30100765346761,7.0738237705915));
#14568=CARTESIAN_POINT('Ctrl Pts',(-14.0883288583003,8.6022976718347,7.11087081976784));
#14569=CARTESIAN_POINT('Ctrl Pts',(-13.6264256690369,8.90358769020179,7.14791786894418));
#14570=CARTESIAN_POINT('Ctrl Pts',(-13.3286453996698,9.45651560934587,7.18496491812052));
#14571=CARTESIAN_POINT('Ctrl Pts',(-13.3312770902519,10.0079748626876,7.22201196729686));
#14572=CARTESIAN_POINT('Ctrl Pts',(-13.333908780834,10.5594341160293,7.2590590164732));
#14573=CARTESIAN_POINT('Ctrl Pts',(-13.6369524313653,11.1094247035687,7.29610606564955));
#14574=CARTESIAN_POINT('Ctrl Pts',(-14.1017092135812,11.4063089541492,7.33315311482589));
#14575=CARTESIAN_POINT('Ctrl Pts',(-14.5664659957971,11.7031932047297,7.37020016400223));
#14576=CARTESIAN_POINT('Ctrl Pts',(-15.1929359096976,11.7469711183514,7.40724721317856));
#14577=CARTESIAN_POINT('Ctrl Pts',(-15.6943994429207,11.5174471764597,7.4442942623549));
#14578=CARTESIAN_POINT('Ctrl Pts',(-16.1958629761437,11.287923234568,7.48134131153124));
#14579=CARTESIAN_POINT('Ctrl Pts',(-16.5723201286892,10.7850974371629,7.51838836070758));
#14580=CARTESIAN_POINT('Ctrl Pts',(-16.6514672347769,10.2394121432165,7.55543540988392));
#14581=CARTESIAN_POINT('Ctrl Pts',(-16.6628933507166,10.1606339826064,7.56078372771935));
#14582=CARTESIAN_POINT('Ctrl Pts',(-16.6681231050028,10.080962569501,7.56613204555478));
#14583=CARTESIAN_POINT('Ctrl Pts',(-16.6674569633666,10.0012065537184,7.57148036339021));
#14584=CARTESIAN_POINT('Ctrl Pts',(-15.5301702171886,8.01482567432828,8.));
#14585=CARTESIAN_POINT('Ctrl Pts',(-16.1903072548812,8.1911250512252,7.96295295082366));
#14586=CARTESIAN_POINT('Ctrl Pts',(-17.3094430093426,9.25114168831851,7.88885885247098));
#14587=CARTESIAN_POINT('Ctrl Pts',(-16.8810963203827,11.5386107605189,7.77771770494196));
#14588=CARTESIAN_POINT('Ctrl Pts',(-14.7276622354211,12.4126888235087,7.66657655741294));
#14589=CARTESIAN_POINT('Ctrl Pts',(-12.8251333276493,11.0807508020576,7.55543540988392));
#14590=CARTESIAN_POINT('Ctrl Pts',(-12.9125602025977,8.75827697936691,7.4442942623549));
#14591=CARTESIAN_POINT('Ctrl Pts',(-14.9111754557965,7.5730758609676,7.33315311482589));
#14592=CARTESIAN_POINT('Ctrl Pts',(-16.9908761101702,8.6090506269142,7.22201196729686));
#14593=CARTESIAN_POINT('Ctrl Pts',(-17.2483215538839,10.9184180559112,7.11087081976785));
#14594=CARTESIAN_POINT('Ctrl Pts',(-15.447683477411,12.3870128478829,6.99972967223881));
#14595=CARTESIAN_POINT('Ctrl Pts',(-13.2372840161297,11.670676405265,6.88858852470981));
#14596=CARTESIAN_POINT('Ctrl Pts',(-12.6403894048645,9.42504512087116,6.77744737718078));
#14597=CARTESIAN_POINT('Ctrl Pts',(-14.2033971295295,7.70571703676082,6.66630622965177));
#14598=CARTESIAN_POINT('Ctrl Pts',(-16.4955794550137,8.08647855754376,6.55516508212274));
#14599=CARTESIAN_POINT('Ctrl Pts',(-17.4187696292973,10.218805211767,6.44402393459373));
#14600=CARTESIAN_POINT('Ctrl Pts',(-16.1279126020198,12.1508445448559,6.33288278706471));
#14601=CARTESIAN_POINT('Ctrl Pts',(-13.8046095450231,12.114086684316,6.22174163953567));
#14602=CARTESIAN_POINT('Ctrl Pts',(-12.5755193539972,10.1421770075384,6.11060049200667));
#14603=CARTESIAN_POINT('Ctrl Pts',(-13.5657030451356,8.04012435007543,5.99945934447765));
#14604=CARTESIAN_POINT('Ctrl Pts',(-15.8687853839106,7.73206425811983,5.88831819694862));
#14605=CARTESIAN_POINT('Ctrl Pts',(-17.3766159710247,9.4999829410875,5.7771770494196));
#14606=CARTESIAN_POINT('Ctrl Pts',(-16.7089862387355,11.7255974394772,5.66603590189059));
#14607=CARTESIAN_POINT('Ctrl Pts',(-14.4770180804847,12.3716682810349,5.55489475436156));
#14608=CARTESIAN_POINT('Ctrl Pts',(-12.7237668892609,10.8468077355158,5.44375360683255));
#14609=CARTESIAN_POINT('Ctrl Pts',(-13.0540894977656,8.54681287249504,5.33261245930352));
#14610=CARTESIAN_POINT('Ctrl Pts',(-15.1656216453787,7.57700805081118,5.22147131177451));
#14611=CARTESIAN_POINT('Ctrl Pts',(-17.1255502875653,8.82511426562272,5.11033016424548));
#14612=CARTESIAN_POINT('Ctrl Pts',(-17.139834231474,11.1486644310237,4.99918901671647));
#14613=CARTESIAN_POINT('Ctrl Pts',(-15.195398520178,12.4207725899548,4.88804786918745));
#14614=CARTESIAN_POINT('Ctrl Pts',(-13.0721027286448,11.4770012270902,4.77690672165843));
#14615=CARTESIAN_POINT('Ctrl Pts',(-12.7135278783817,9.18124133547139,4.66576557412941));
#14616=CARTESIAN_POINT('Ctrl Pts',(-14.4478992106895,7.63494075503149,4.55462442660039));
#14617=CARTESIAN_POINT('Ctrl Pts',(-16.687641777794,8.25352190292165,4.44348327907136));
#14618=CARTESIAN_POINT('Ctrl Pts',(-17.3825837837853,10.4707600524374,4.33234213154235));
#14619=CARTESIAN_POINT('Ctrl Pts',(-15.8966027914863,12.2570830618385,4.22120098401332));
#14620=CARTESIAN_POINT('Ctrl Pts',(-13.5899070517775,11.9773614720396,4.11005983648431));
#14621=CARTESIAN_POINT('Ctrl Pts',(-12.5739546477039,9.8876413673274,3.99891868895528));
#14622=CARTESIAN_POINT('Ctrl Pts',(-13.7787082434502,7.90076991277298,3.88777754142627));
#14623=CARTESIAN_POINT('Ctrl Pts',(-16.1013840283822,7.83545068530234,3.77663639389724));
#14624=CARTESIAN_POINT('Ctrl Pts',(-17.4158964178437,9.75147432329159,3.66549524636823));
#14625=CARTESIAN_POINT('Ctrl Pts',(-16.518992740837,11.8949885400772,3.5543540988392));
#14626=CARTESIAN_POINT('Ctrl Pts',(-14.2316631634768,12.3039051671823,3.44321295131019));
#14627=CARTESIAN_POINT('Ctrl Pts',(-12.647638749453,10.6039180910149,3.33207180378117));
#14628=CARTESIAN_POINT('Ctrl Pts',(-13.2168728216632,8.35112827071217,3.22093065625215));
#14629=CARTESIAN_POINT('Ctrl Pts',(-15.4183110155551,7.60765044194128,3.10978950872313));
#14630=CARTESIAN_POINT('Ctrl Pts',(-17.2368438440502,9.05403481509122,2.99864836119411));
#14631=CARTESIAN_POINT('Ctrl Pts',(-17.0078582531826,11.3663183190935,2.88750721366509));
#14632=CARTESIAN_POINT('Ctrl Pts',(-14.9409585995702,12.4279280521305,2.77636606613606));
#14633=CARTESIAN_POINT('Ctrl Pts',(-12.9281031098292,11.2671084366828,2.66522491860705));
#14634=CARTESIAN_POINT('Ctrl Pts',(-12.8117801189011,8.94642785381579,2.55408377107803));
#14635=CARTESIAN_POINT('Ctrl Pts',(-14.6984670947123,7.59014556097653,2.44294262354901));
#14636=CARTESIAN_POINT('Ctrl Pts',(-16.8611653694553,8.43974874366516,2.33180147601999));
#14637=CARTESIAN_POINT('Ctrl Pts',(-17.3202264500472,10.7175442452619,2.22066032849097));
#14638=CARTESIAN_POINT('Ctrl Pts',(-15.655443965717,12.3385281044116,2.10951918096195));
#14639=CARTESIAN_POINT('Ctrl Pts',(-13.3906939975623,11.8189158098855,1.99837803343293));
#14640=CARTESIAN_POINT('Ctrl Pts',(-12.5990391016035,9.63433986139397,1.88723688590391));
#14641=CARTESIAN_POINT('Ctrl Pts',(-14.0051289214666,7.7844748128269,1.77609573837489));
#14642=CARTESIAN_POINT('Ctrl Pts',(-16.3218843289188,7.96261380065688,1.66495459084587));
#14643=CARTESIAN_POINT('Ctrl Pts',(-17.4286392087695,10.0056958124645,1.55381344331685));
#14644=CARTESIAN_POINT('Ctrl Pts',(-16.3123135322607,12.0435636244015,1.44267229578783));
#14645=CARTESIAN_POINT('Ctrl Pts',(-13.9947484023904,12.2108350155113,1.33153114825881));
#14646=CARTESIAN_POINT('Ctrl Pts',(-12.5973499293358,10.3543936440402,1.22039000072979));
#14647=CARTESIAN_POINT('Ctrl Pts',(-13.3992441080921,8.17355782375309,1.10924885320077));
#14648=CARTESIAN_POINT('Ctrl Pts',(-15.6664035170272,7.66456821418318,0.998107705671752));
#14649=CARTESIAN_POINT('Ctrl Pts',(-17.323570133058,9.29335360493268,0.886966558142732));
#14650=CARTESIAN_POINT('Ctrl Pts',(-16.8538196455965,11.5689498250439,0.775825410613712));
#14651=CARTESIAN_POINT('Ctrl Pts',(-14.6871808849242,12.408440519574,0.664684263084692));
#14652=CARTESIAN_POINT('Ctrl Pts',(-12.8068360443054,11.0432447977232,0.553543115555672));
#14653=CARTESIAN_POINT('Ctrl Pts',(-12.9341204463425,8.72328850320409,0.442401968026654));
#14654=CARTESIAN_POINT('Ctrl Pts',(-14.9522477729176,7.57162591585277,0.331260820497632));
#14655=CARTESIAN_POINT('Ctrl Pts',(-17.0144376022166,8.64349401570581,0.220119672968612));
#14656=CARTESIAN_POINT('Ctrl Pts',(-17.2320070103418,10.9557091204361,0.108978525439593));
#14657=CARTESIAN_POINT('Ctrl Pts',(-15.4078276845629,12.3957301639888,-0.00216262208942797));
#14658=CARTESIAN_POINT('Ctrl Pts',(-13.2075704878879,11.6375323595232,-0.113303769618446));
#14659=CARTESIAN_POINT('Ctrl Pts',(-12.839200671623,10.1407345153594,-0.187397867971127));
#14660=CARTESIAN_POINT('Ctrl Pts',(-13.0122087991468,9.47972727890995,-0.224444917147467));
#14661=CARTESIAN_POINT('Ctrl Pts',(-15.4967348970877,8.14002119999723,8.07481497238249));
#14662=CARTESIAN_POINT('Ctrl Pts',(-16.1152402239634,8.30520221168044,8.03776792320615));
#14663=CARTESIAN_POINT('Ctrl Pts',(-17.1637973963513,9.29836862893029,7.96367382485347));
#14664=CARTESIAN_POINT('Ctrl Pts',(-16.7624645006887,11.4415778800953,7.85253267732445));
#14665=CARTESIAN_POINT('Ctrl Pts',(-14.7448372860729,12.260531986888,7.74139152979543));
#14666=CARTESIAN_POINT('Ctrl Pts',(-12.9622918495906,11.0125929768072,7.63025038226641));
#14667=CARTESIAN_POINT('Ctrl Pts',(-13.04420512635,8.83658655867844,7.5191092347374));
#14668=CARTESIAN_POINT('Ctrl Pts',(-14.9167771983538,7.72613045139609,7.40796808720836));
#14669=CARTESIAN_POINT('Ctrl Pts',(-16.8653210000062,8.69677120424107,7.29682693967935));
#14670=CARTESIAN_POINT('Ctrl Pts',(-17.1065305810855,10.8604977867405,7.18568579215034));
#14671=CARTESIAN_POINT('Ctrl Pts',(-15.4194502046132,12.2364752732202,7.07454464462131));
#14672=CARTESIAN_POINT('Ctrl Pts',(-13.3484501496788,11.5653147712387,6.96340349709229));
#14673=CARTESIAN_POINT('Ctrl Pts',(-12.7891988494618,9.461304797111,6.85226234956327));
#14674=CARTESIAN_POINT('Ctrl Pts',(-14.2536350929307,7.85040657757425,6.74112120203425));
#14675=CARTESIAN_POINT('Ctrl Pts',(-16.4012603548577,8.20715527583956,6.62998005450523));
#14676=CARTESIAN_POINT('Ctrl Pts',(-17.2662293051071,10.2050062052253,6.51883890697622));
#14677=CARTESIAN_POINT('Ctrl Pts',(-16.0567805058142,12.0152009845181,6.40769775944719));
#14678=CARTESIAN_POINT('Ctrl Pts',(-13.8799971492527,11.9807612678375,6.29655661191817));
#14679=CARTESIAN_POINT('Ctrl Pts',(-12.7284198449139,10.1332105782598,6.18541546438915));
#14680=CARTESIAN_POINT('Ctrl Pts',(-13.6561573487741,8.16372440829958,6.07427431686013));
#14681=CARTESIAN_POINT('Ctrl Pts',(-15.813995211871,7.87509220469174,5.96313316933111));
#14682=CARTESIAN_POINT('Ctrl Pts',(-17.2267340780554,9.53151664456354,5.8519920218021));
#14683=CARTESIAN_POINT('Ctrl Pts',(-16.6012085852808,11.6167721964068,5.74085087427307));
#14684=CARTESIAN_POINT('Ctrl Pts',(-14.5100000687576,12.222098415398,5.62970972674406));
#14685=CARTESIAN_POINT('Ctrl Pts',(-12.8673181115183,10.7934035894831,5.51856857921503));
#14686=CARTESIAN_POINT('Ctrl Pts',(-13.1768088403853,8.63845848969381,5.40742743168602));
#14687=CARTESIAN_POINT('Ctrl Pts',(-15.1551766740293,7.72981465668329,5.296286284157));
#14688=CARTESIAN_POINT('Ctrl Pts',(-16.9915019160211,8.89920873441279,5.18514513662797));
#14689=CARTESIAN_POINT('Ctrl Pts',(-17.0048850393605,11.076223615424,5.07400398909895));
#14690=CARTESIAN_POINT('Ctrl Pts',(-15.1830756626172,12.2681059485394,4.96286284156994));
#14691=CARTESIAN_POINT('Ctrl Pts',(-13.1936860622603,11.3838537676213,4.85172169404091));
#14692=CARTESIAN_POINT('Ctrl Pts',(-12.8577248264742,9.23287655968122,4.74058054651189));
#14693=CARTESIAN_POINT('Ctrl Pts',(-14.4827175879203,7.78409382012157,4.62943939898288));
#14694=CARTESIAN_POINT('Ctrl Pts',(-16.5812102182179,8.36366398999456,4.51829825145385));
#14695=CARTESIAN_POINT('Ctrl Pts',(-17.2323255291807,10.4410714495441,4.40715710392484));
#14696=CARTESIAN_POINT('Ctrl Pts',(-15.8400583075361,12.1147395423041,4.29601595639581));
#14697=CARTESIAN_POINT('Ctrl Pts',(-13.6788349235578,11.8526586659796,4.1848748088668));
#14698=CARTESIAN_POINT('Ctrl Pts',(-12.7269538172226,9.89472729318237,4.07373366133777));
#14699=CARTESIAN_POINT('Ctrl Pts',(-13.8557293198762,8.03315839416316,3.96259251380876));
#14700=CARTESIAN_POINT('Ctrl Pts',(-16.0319249634459,7.97195854044916,3.85145136627973));
#14701=CARTESIAN_POINT('Ctrl Pts',(-17.2635372934674,9.76714765854248,3.74031021875072));
#14702=CARTESIAN_POINT('Ctrl Pts',(-16.423197075833,11.7754806040014,3.62916907122169));
#14703=CARTESIAN_POINT('Ctrl Pts',(-14.2801185222307,12.1586087996206,3.51802792369268));
#14704=CARTESIAN_POINT('Ctrl Pts',(-12.795991012283,10.5658318424231,3.40688677616365));
#14705=CARTESIAN_POINT('Ctrl Pts',(-13.3293261924023,8.45511478728119,3.29574562863464));
#14706=CARTESIAN_POINT('Ctrl Pts',(-15.3919301245631,7.7585245775937,3.18460448110562));
#14707=CARTESIAN_POINT('Ctrl Pts',(-17.0957767159528,9.113692350985,3.0734633335766));
#14708=CARTESIAN_POINT('Ctrl Pts',(-16.8812321598339,11.2801511054751,2.96232218604758));
#14709=CARTESIAN_POINT('Ctrl Pts',(-14.9446820605617,12.2748101496661,2.85118103851856));
#14710=CARTESIAN_POINT('Ctrl Pts',(-13.0587678161688,11.1871979196271,2.74003989098954));
#14711=CARTESIAN_POINT('Ctrl Pts',(-12.9497807643611,9.01287165019477,2.62889874346052));
#14712=CARTESIAN_POINT('Ctrl Pts',(-14.7174833443665,7.74212364641602,2.5177575959315));
#14713=CARTESIAN_POINT('Ctrl Pts',(-16.74379050027,8.53814638748237,2.40661644840248));
#14714=CARTESIAN_POINT('Ctrl Pts',(-17.1739007766148,10.6722921342434,2.29547530087346));
#14715=CARTESIAN_POINT('Ctrl Pts',(-15.6141082246824,12.1910482324743,2.18433415334444));
#14716=CARTESIAN_POINT('Ctrl Pts',(-13.4921852914663,11.7042054199608,2.07319300581542));
#14717=CARTESIAN_POINT('Ctrl Pts',(-12.7504563136328,9.65740031138922,1.9620518582864));
#14718=CARTESIAN_POINT('Ctrl Pts',(-14.0678707200277,7.92419747438564,1.85091071075738));
#14719=CARTESIAN_POINT('Ctrl Pts',(-16.2385193562348,8.09110208146877,1.73976956322836));
#14720=CARTESIAN_POINT('Ctrl Pts',(-17.2754764570301,10.0053366045973,1.62862841569934));
#14721=CARTESIAN_POINT('Ctrl Pts',(-16.2295521443114,11.9146857627012,1.51748726817032));
#14722=CARTESIAN_POINT('Ctrl Pts',(-14.0581448510371,12.0714081408258,1.4063461206413));
#14723=CARTESIAN_POINT('Ctrl Pts',(-12.7488736694455,10.3320437184011,1.29520497311228));
#14724=CARTESIAN_POINT('Ctrl Pts',(-13.5001961870926,8.28874286589384,1.18406382558326));
#14725=CARTESIAN_POINT('Ctrl Pts',(-15.6243766090913,7.81185281599787,1.07292267805424));
#14726=CARTESIAN_POINT('Ctrl Pts',(-17.1770335894029,9.33791844024638,0.961781530525221));
#14727=CARTESIAN_POINT('Ctrl Pts',(-16.7369080363618,11.4700036037703,0.8506403829962));
#14728=CARTESIAN_POINT('Ctrl Pts',(-14.70690890228,12.2565516033255,0.739499235467183));
#14729=CARTESIAN_POINT('Ctrl Pts',(-12.9451484890921,10.9774522982115,0.628358087938161));
#14730=CARTESIAN_POINT('Ctrl Pts',(-13.0644056678186,8.80380463969748,0.517216940409144));
#14731=CARTESIAN_POINT('Ctrl Pts',(-14.9552592793098,7.72477194744011,0.406075792880121));
#14732=CARTESIAN_POINT('Ctrl Pts',(-16.8873965805413,8.72904241192503,0.294934645351101));
#14733=CARTESIAN_POINT('Ctrl Pts',(-17.0912449183971,10.8954370807606,0.183793497822082));
#14734=CARTESIAN_POINT('Ctrl Pts',(-15.3821079275164,12.2446428295604,0.0726523502930611));
#14735=CARTESIAN_POINT('Ctrl Pts',(-13.3206105126815,11.5342609632034,-0.0384887972359573));
#14736=CARTESIAN_POINT('Ctrl Pts',(-12.9754720329252,10.1318590572183,-0.112582895588638));
#14737=CARTESIAN_POINT('Ctrl Pts',(-13.1375693587171,9.51253841089255,-0.149629944764978));
#14738=CARTESIAN_POINT('Ctrl Pts',(-15.4632995769868,8.26521672566619,8.14962994476498));
#14739=CARTESIAN_POINT('Ctrl Pts',(-16.0401731930456,8.41927937213568,8.11258289558864));
#14740=CARTESIAN_POINT('Ctrl Pts',(-17.0181517833599,9.34559556954207,8.03848879723596));
#14741=CARTESIAN_POINT('Ctrl Pts',(-16.6438326809947,11.3445449996716,7.92734764970694));
#14742=CARTESIAN_POINT('Ctrl Pts',(-14.7620123367246,12.1083751502674,7.81620650217792));
#14743=CARTESIAN_POINT('Ctrl Pts',(-13.0994503715318,10.9444351515568,7.7050653546489));
#14744=CARTESIAN_POINT('Ctrl Pts',(-13.1758500501023,8.91489613798999,7.59392420711989));
#14745=CARTESIAN_POINT('Ctrl Pts',(-14.9223789409112,7.87918504182458,7.48278305959085));
#14746=CARTESIAN_POINT('Ctrl Pts',(-16.7397658898422,8.78449178156794,7.37164191206185));
#14747=CARTESIAN_POINT('Ctrl Pts',(-16.9647396082871,10.8025775175698,7.26050076453282));
#14748=CARTESIAN_POINT('Ctrl Pts',(-15.3912169318155,12.0859376985576,7.1493596170038));
#14749=CARTESIAN_POINT('Ctrl Pts',(-13.4596162832278,11.4599531372124,7.03821846947478));
#14750=CARTESIAN_POINT('Ctrl Pts',(-12.9380082940591,9.49756447335083,6.92707732194576));
#14751=CARTESIAN_POINT('Ctrl Pts',(-14.3038730563318,7.99509611838767,6.81593617441674));
#14752=CARTESIAN_POINT('Ctrl Pts',(-16.3069412547017,8.32783199413537,6.70479502688772));
#14753=CARTESIAN_POINT('Ctrl Pts',(-17.113688980917,10.1912071986836,6.5936538793587));
#14754=CARTESIAN_POINT('Ctrl Pts',(-15.9856484096087,11.8795574241802,6.48251273182968));
#14755=CARTESIAN_POINT('Ctrl Pts',(-13.9553847534823,11.8474358513589,6.37137158430066));
#14756=CARTESIAN_POINT('Ctrl Pts',(-12.8813203358307,10.1242441489812,6.26023043677164));
#14757=CARTESIAN_POINT('Ctrl Pts',(-13.7466116524126,8.28732446652372,6.14908928924262));
#14758=CARTESIAN_POINT('Ctrl Pts',(-15.7592050398313,8.01812015126366,6.0379481417136));
#14759=CARTESIAN_POINT('Ctrl Pts',(-17.0768521850862,9.56305034803959,5.92680699418459));
#14760=CARTESIAN_POINT('Ctrl Pts',(-16.4934309318261,11.5079469533364,5.81566584665556));
#14761=CARTESIAN_POINT('Ctrl Pts',(-14.5429820570306,12.0725285497611,5.70452469912655));
#14762=CARTESIAN_POINT('Ctrl Pts',(-13.0108693337756,10.7399994434505,5.59338355159753));
#14763=CARTESIAN_POINT('Ctrl Pts',(-13.299528183005,8.73010410689258,5.4822424040685));
#14764=CARTESIAN_POINT('Ctrl Pts',(-15.1447317026798,7.8826212625554,5.37110125653949));
#14765=CARTESIAN_POINT('Ctrl Pts',(-16.857453544477,8.97330320320286,5.25996010901046));
#14766=CARTESIAN_POINT('Ctrl Pts',(-16.869935847247,11.0037827998243,5.14881896148144));
#14767=CARTESIAN_POINT('Ctrl Pts',(-15.1707528050564,12.115439307124,5.03767781395243));
#14768=CARTESIAN_POINT('Ctrl Pts',(-13.3152693958758,11.2907063081524,4.9265366664234));
#14769=CARTESIAN_POINT('Ctrl Pts',(-13.0019217745667,9.28451178389106,4.81539551889439));
#14770=CARTESIAN_POINT('Ctrl Pts',(-14.517535965151,7.93324688521165,4.70425437136536));
#14771=CARTESIAN_POINT('Ctrl Pts',(-16.4747786586417,8.47380607706747,4.59311322383635));
#14772=CARTESIAN_POINT('Ctrl Pts',(-17.082067274576,10.4113828466508,4.48197207630732));
#14773=CARTESIAN_POINT('Ctrl Pts',(-15.7835138235858,11.9723960227698,4.3708309287783));
#14774=CARTESIAN_POINT('Ctrl Pts',(-13.7677627953381,11.7279558599196,4.25968978124929));
#14775=CARTESIAN_POINT('Ctrl Pts',(-12.8799529867411,9.90181321903733,4.14854863372026));
#14776=CARTESIAN_POINT('Ctrl Pts',(-13.9327503963021,8.16554687555337,4.03740748619125));
#14777=CARTESIAN_POINT('Ctrl Pts',(-15.9624658985096,8.10846639559596,3.92626633866222));
#14778=CARTESIAN_POINT('Ctrl Pts',(-17.1111781690911,9.78282099379339,3.81512519113321));
#14779=CARTESIAN_POINT('Ctrl Pts',(-16.3274014108291,11.6559726679257,3.70398404360419));
#14780=CARTESIAN_POINT('Ctrl Pts',(-14.3285738809845,12.0133124320589,3.59284289607517));
#14781=CARTESIAN_POINT('Ctrl Pts',(-12.9443432751131,10.5277455938313,3.48170174854614));
#14782=CARTESIAN_POINT('Ctrl Pts',(-13.4417795631413,8.55910130385022,3.37056060101713));
#14783=CARTESIAN_POINT('Ctrl Pts',(-15.3655492335712,7.90939871324609,3.2594194534881));
#14784=CARTESIAN_POINT('Ctrl Pts',(-16.9547095878554,9.17334988687881,3.14827830595909));
#14785=CARTESIAN_POINT('Ctrl Pts',(-16.7546060664852,11.1939838918566,3.03713715843006));
#14786=CARTESIAN_POINT('Ctrl Pts',(-14.9484055215533,12.1216922472018,2.92599601090105));
#14787=CARTESIAN_POINT('Ctrl Pts',(-13.1894325225084,11.1072874025715,2.81485486337203));
#14788=CARTESIAN_POINT('Ctrl Pts',(-13.0877814098212,9.07931544657375,2.703713715843));
#14789=CARTESIAN_POINT('Ctrl Pts',(-14.7364995940206,7.8941017318555,2.59257256831399));
#14790=CARTESIAN_POINT('Ctrl Pts',(-16.6264156310847,8.63654403129957,2.48143142078497));
#14791=CARTESIAN_POINT('Ctrl Pts',(-17.0275751031823,10.627040023225,2.37029027325595));
#14792=CARTESIAN_POINT('Ctrl Pts',(-15.5727724836478,12.0435683605368,2.25914912572693));
#14793=CARTESIAN_POINT('Ctrl Pts',(-13.5936765853703,11.5894950300362,2.14800797819791));
#14794=CARTESIAN_POINT('Ctrl Pts',(-12.9018735256621,9.68046076138442,2.03686683066889));
#14795=CARTESIAN_POINT('Ctrl Pts',(-14.1306125185887,8.06392013594442,1.92572568313987));
#14796=CARTESIAN_POINT('Ctrl Pts',(-16.1551543835509,8.21959036228063,1.81458453561085));
#14797=CARTESIAN_POINT('Ctrl Pts',(-17.1223137052908,10.0049773967301,1.70344338808183));
#14798=CARTESIAN_POINT('Ctrl Pts',(-16.1467907563622,11.7858079010009,1.59230224055281));
#14799=CARTESIAN_POINT('Ctrl Pts',(-14.1215412996839,11.9319812661403,1.48116109302379));
#14800=CARTESIAN_POINT('Ctrl Pts',(-12.900397409555,10.3096937927621,1.37001994549477));
#14801=CARTESIAN_POINT('Ctrl Pts',(-13.6011482660932,8.40392790803455,1.25887879796575));
#14802=CARTESIAN_POINT('Ctrl Pts',(-15.5823497011553,7.95913741781259,1.14773765043673));
#14803=CARTESIAN_POINT('Ctrl Pts',(-17.0304970457477,9.38248327556005,1.03659650290771));
#14804=CARTESIAN_POINT('Ctrl Pts',(-16.6199964271269,11.3710573824967,0.925455355378691));
#14805=CARTESIAN_POINT('Ctrl Pts',(-14.7266369196359,12.1046626870771,0.814314207849671));
#14806=CARTESIAN_POINT('Ctrl Pts',(-13.0834609338788,10.9116597986998,0.70317306032065));
#14807=CARTESIAN_POINT('Ctrl Pts',(-13.1946908892948,8.88432077619087,0.592031912791632));
#14808=CARTESIAN_POINT('Ctrl Pts',(-14.958270785702,7.87791797902744,0.48089076526261));
#14809=CARTESIAN_POINT('Ctrl Pts',(-16.760355558866,8.81459080814426,0.36974961773359));
#14810=CARTESIAN_POINT('Ctrl Pts',(-16.9504828264524,10.8351650410851,0.258608470204571));
#14811=CARTESIAN_POINT('Ctrl Pts',(-15.3563881704699,12.0935554951319,0.14746732267555));
#14812=CARTESIAN_POINT('Ctrl Pts',(-13.433650537475,11.4309895668835,0.0363261751465318));
#14813=CARTESIAN_POINT('Ctrl Pts',(-13.1117433942273,10.1229835990773,-0.0377679232061492));
#14814=CARTESIAN_POINT('Ctrl Pts',(-13.2629299182875,9.54534954287515,-0.0748149723824891));
#14815=CARTESIAN_POINT('Ctrl Pts',(-15.4298642568859,8.39041225133515,8.22444491714747));
#14816=CARTESIAN_POINT('Ctrl Pts',(-15.9651061621278,8.53335653259092,8.18739786797113));
#14817=CARTESIAN_POINT('Ctrl Pts',(-16.8725061703686,9.39282251015386,8.11330376961845));
#14818=CARTESIAN_POINT('Ctrl Pts',(-16.5252008613007,11.2475121192479,8.00216262208942));
#14819=CARTESIAN_POINT('Ctrl Pts',(-14.7791873873764,11.9562183136467,7.89102147456041));
#14820=CARTESIAN_POINT('Ctrl Pts',(-13.236608893473,10.8762773263063,7.77988032703139));
#14821=CARTESIAN_POINT('Ctrl Pts',(-13.3074949738546,8.99320571730152,7.66873917950237));
#14822=CARTESIAN_POINT('Ctrl Pts',(-14.9279806834685,8.03223963225308,7.55759803197335));
#14823=CARTESIAN_POINT('Ctrl Pts',(-16.6142107796781,8.87221235889479,7.44645688444433));
#14824=CARTESIAN_POINT('Ctrl Pts',(-16.8229486354888,10.7446572483991,7.33531573691531));
#14825=CARTESIAN_POINT('Ctrl Pts',(-15.3629836590177,11.9354001238949,7.22417458938629));
#14826=CARTESIAN_POINT('Ctrl Pts',(-13.5707824167768,11.3545915031861,7.11303344185727));
#14827=CARTESIAN_POINT('Ctrl Pts',(-13.0868177386564,9.53382414959064,7.00189229432825));
#14828=CARTESIAN_POINT('Ctrl Pts',(-14.3541110197329,8.13978565920112,6.89075114679923));
#14829=CARTESIAN_POINT('Ctrl Pts',(-16.2126221545457,8.44850871243116,6.77960999927022));
#14830=CARTESIAN_POINT('Ctrl Pts',(-16.9611486567268,10.177408192142,6.66846885174119));
#14831=CARTESIAN_POINT('Ctrl Pts',(-15.9145163134031,11.7439138638423,6.55732770421217));
#14832=CARTESIAN_POINT('Ctrl Pts',(-14.0307723577119,11.7141104348804,6.44618655668315));
#14833=CARTESIAN_POINT('Ctrl Pts',(-13.0342208267474,10.1152777197026,6.33504540915413));
#14834=CARTESIAN_POINT('Ctrl Pts',(-13.8370659560511,8.41092452474786,6.22390426162511));
#14835=CARTESIAN_POINT('Ctrl Pts',(-15.7044148677917,8.16114809783556,6.11276311409609));
#14836=CARTESIAN_POINT('Ctrl Pts',(-16.9269702921169,9.59458405151565,6.00162196656707));
#14837=CARTESIAN_POINT('Ctrl Pts',(-16.3856532783713,11.399121710266,5.89048081903805));
#14838=CARTESIAN_POINT('Ctrl Pts',(-14.5759640453036,11.9229586841242,5.77933967150902));
#14839=CARTESIAN_POINT('Ctrl Pts',(-13.154420556033,10.6865952974178,5.66819852398002));
#14840=CARTESIAN_POINT('Ctrl Pts',(-13.4222475256247,8.82174972409137,5.55705737645099));
#14841=CARTESIAN_POINT('Ctrl Pts',(-15.1342867313303,8.0354278684275,5.44591622892198));
#14842=CARTESIAN_POINT('Ctrl Pts',(-16.7234051729329,9.04739767199292,5.33477508139295));
#14843=CARTESIAN_POINT('Ctrl Pts',(-16.7349866551335,10.9313419842246,5.22363393386394));
#14844=CARTESIAN_POINT('Ctrl Pts',(-15.1584299474956,11.9627726657085,5.11249278633491));
#14845=CARTESIAN_POINT('Ctrl Pts',(-13.4368527294913,11.1975588486834,5.00135163880589));
#14846=CARTESIAN_POINT('Ctrl Pts',(-13.1461187226592,9.3361470081009,4.89021049127687));
#14847=CARTESIAN_POINT('Ctrl Pts',(-14.5523543423817,8.08239995030172,4.77906934374785));
#14848=CARTESIAN_POINT('Ctrl Pts',(-16.3683470990655,8.58394816414039,4.66792819621883));
#14849=CARTESIAN_POINT('Ctrl Pts',(-16.9318090199714,10.3816942437575,4.55678704868981));
#14850=CARTESIAN_POINT('Ctrl Pts',(-15.7269693396356,11.8300525032354,4.44564590116079));
#14851=CARTESIAN_POINT('Ctrl Pts',(-13.8566906671183,11.6032530538596,4.33450475363177));
#14852=CARTESIAN_POINT('Ctrl Pts',(-13.0329521562598,9.90889914489231,4.22336360610275));
#14853=CARTESIAN_POINT('Ctrl Pts',(-14.0097714727281,8.29793535694355,4.11222245857373));
#14854=CARTESIAN_POINT('Ctrl Pts',(-15.8930068335733,8.24497425074277,4.00108131104471));
#14855=CARTESIAN_POINT('Ctrl Pts',(-16.9588190447147,9.7984943290443,3.8899401635157));
#14856=CARTESIAN_POINT('Ctrl Pts',(-16.2316057458252,11.5364647318499,3.77879901598667));
#14857=CARTESIAN_POINT('Ctrl Pts',(-14.3770292397384,11.8680160644972,3.66765786845765));
#14858=CARTESIAN_POINT('Ctrl Pts',(-13.0926955379431,10.4896593452395,3.55651672092863));
#14859=CARTESIAN_POINT('Ctrl Pts',(-13.5542329338804,8.66308782041927,3.44537557339962));
#14860=CARTESIAN_POINT('Ctrl Pts',(-15.3391683425793,8.06027284889848,3.33423442587059));
#14861=CARTESIAN_POINT('Ctrl Pts',(-16.813642459758,9.2330074227726,3.22309327834158));
#14862=CARTESIAN_POINT('Ctrl Pts',(-16.6279799731365,11.1078166782381,3.11195213081255));
#14863=CARTESIAN_POINT('Ctrl Pts',(-14.9521289825448,11.9685743447375,3.00081098328354));
#14864=CARTESIAN_POINT('Ctrl Pts',(-13.320097228848,11.0273768855158,2.88966983575452));
#14865=CARTESIAN_POINT('Ctrl Pts',(-13.2257820552813,9.14575924295271,2.77852868822549));
#14866=CARTESIAN_POINT('Ctrl Pts',(-14.7555158436747,8.046079817295,2.66738754069648));
#14867=CARTESIAN_POINT('Ctrl Pts',(-16.5090407618993,8.73494167511676,2.55624639316746));
#14868=CARTESIAN_POINT('Ctrl Pts',(-16.8812494297499,10.5817879122065,2.44510524563843));
#14869=CARTESIAN_POINT('Ctrl Pts',(-15.5314367426132,11.8960884885995,2.33396409810942));
#14870=CARTESIAN_POINT('Ctrl Pts',(-13.6951678792743,11.4747846401115,2.22282295058039));
#14871=CARTESIAN_POINT('Ctrl Pts',(-13.0532907376914,9.70352121137968,2.11168180305138));
#14872=CARTESIAN_POINT('Ctrl Pts',(-14.1933543171498,8.20364279750315,2.00054065552236));
#14873=CARTESIAN_POINT('Ctrl Pts',(-16.0717894108669,8.34807864309253,1.88939950799334));
#14874=CARTESIAN_POINT('Ctrl Pts',(-16.9691509535515,10.0046181888628,1.77825836046432));
#14875=CARTESIAN_POINT('Ctrl Pts',(-16.0640293684129,11.6569300393006,1.6671172129353));
#14876=CARTESIAN_POINT('Ctrl Pts',(-14.1849377483306,11.7925543914548,1.55597606540628));
#14877=CARTESIAN_POINT('Ctrl Pts',(-13.0519211496647,10.287343867123,1.44483491787726));
#14878=CARTESIAN_POINT('Ctrl Pts',(-13.7021003450938,8.51911295017527,1.33369377034824));
#14879=CARTESIAN_POINT('Ctrl Pts',(-15.5403227932193,8.1064220196273,1.22255262281922));
#14880=CARTESIAN_POINT('Ctrl Pts',(-16.8839605020926,9.42704811087374,1.1114114752902));
#14881=CARTESIAN_POINT('Ctrl Pts',(-16.5030848178921,11.2721111612231,1.00027032776118));
#14882=CARTESIAN_POINT('Ctrl Pts',(-14.7463649369917,11.9527737708287,0.88912918023216));
#14883=CARTESIAN_POINT('Ctrl Pts',(-13.2217733786655,10.8458672991881,0.777988032703139));
#14884=CARTESIAN_POINT('Ctrl Pts',(-13.3249761107709,8.96483691268427,0.666846885174121));
#14885=CARTESIAN_POINT('Ctrl Pts',(-14.9612822920943,8.03106401061478,0.555705737645099));
#14886=CARTESIAN_POINT('Ctrl Pts',(-16.6333145371908,8.90013920436348,0.444564590116079));
#14887=CARTESIAN_POINT('Ctrl Pts',(-16.8097207345076,10.7748930014097,0.33342344258706));
#14888=CARTESIAN_POINT('Ctrl Pts',(-15.3306684134234,11.9424681607034,0.222282295058039));
#14889=CARTESIAN_POINT('Ctrl Pts',(-13.5466905622686,11.3277181705637,0.111141147529021));
#14890=CARTESIAN_POINT('Ctrl Pts',(-13.2480147555294,10.1141081409362,0.0370470491763399));
#14891=CARTESIAN_POINT('Ctrl Pts',(-13.3882904778579,9.57816067485776,0.));
#14892=CARTESIAN_POINT('Ctrl Pts',(-16.6638185641669,10.0009395545784,7.3785196366098));
#14893=CARTESIAN_POINT('Ctrl Pts',(-16.6649347763355,10.2169537916664,7.36411833671164));
#14894=CARTESIAN_POINT('Ctrl Pts',(-16.6258964192002,10.4325814095807,7.34971703681347));
#14895=CARTESIAN_POINT('Ctrl Pts',(-16.5448314967751,10.6310402460644,7.33531573691531));
#14896=CARTESIAN_POINT('Ctrl Pts',(-16.3362936433318,11.141571540231,7.29826868773897));
#14897=CARTESIAN_POINT('Ctrl Pts',(-15.8496386511747,11.538485832063,7.26122163856263));
#14898=CARTESIAN_POINT('Ctrl Pts',(-15.3076109480561,11.6401415411941,7.22417458938629));
#14899=CARTESIAN_POINT('Ctrl Pts',(-14.7655832449374,11.7417972503253,7.18712754020995));
#14900=CARTESIAN_POINT('Ctrl Pts',(-14.1681828308571,11.5481943767557,7.15008049103361));
#14901=CARTESIAN_POINT('Ctrl Pts',(-13.7888218441302,11.1479317143716,7.11303344185727));
#14902=CARTESIAN_POINT('Ctrl Pts',(-13.4094608574033,10.7476690519876,7.07598639268093));
#14903=CARTESIAN_POINT('Ctrl Pts',(-13.2481392980299,10.1407466007891,7.03893934350459));
#14904=CARTESIAN_POINT('Ctrl Pts',(-13.3786940651892,9.60494562679162,7.00189229432825));
#14905=CARTESIAN_POINT('Ctrl Pts',(-13.5092488323486,9.06914465279414,6.96484524515191));
#14906=CARTESIAN_POINT('Ctrl Pts',(-13.9316799260408,8.60446515599763,6.92779819597557));
#14907=CARTESIAN_POINT('Ctrl Pts',(-14.452647328689,8.42357924980438,6.89075114679923));
#14908=CARTESIAN_POINT('Ctrl Pts',(-14.9736147313372,8.24269334361113,6.85370409762289));
#14909=CARTESIAN_POINT('Ctrl Pts',(-15.5931184429414,8.34560102802114,6.81665704844655));
#14910=CARTESIAN_POINT('Ctrl Pts',(-16.0276247157737,8.68520478351129,6.77960999927021));
#14911=CARTESIAN_POINT('Ctrl Pts',(-16.4228374490899,8.99409728252362,6.74591321171674));
#14912=CARTESIAN_POINT('Ctrl Pts',(-16.6649994289874,9.49881147642293,6.71221642416327));
#14913=CARTESIAN_POINT('Ctrl Pts',(-16.6681787596498,10.0008675363463,6.67851963660979));
#14914=CARTESIAN_POINT('Ctrl Pts',(-15.5301702171886,8.01482567432828,8.));
#14915=CARTESIAN_POINT('Ctrl Pts',(-15.6001784828994,8.04074713960098,8.));
#14916=CARTESIAN_POINT('Ctrl Pts',(-15.6685003719384,8.07074116686246,8.));
#14917=CARTESIAN_POINT('Ctrl Pts',(-15.7349165600646,8.10452089866272,8.));
#14918=CARTESIAN_POINT('Ctrl Pts',(-15.7995896602114,8.13741408388292,8.));
#14919=CARTESIAN_POINT('Ctrl Pts',(-15.8624562004235,8.17389779453761,8.));
#14920=CARTESIAN_POINT('Ctrl Pts',(-15.9232827418904,8.2137409613008,8.));
#14921=CARTESIAN_POINT('Ctrl Pts',(-15.9368594118801,8.22263407791475,8.));
#14922=CARTESIAN_POINT('Ctrl Pts',(-15.9503360961863,8.23169590343848,8.));
#14923=CARTESIAN_POINT('Ctrl Pts',(-15.963704238615,8.24092008435083,8.));
#14924=CARTESIAN_POINT('Ctrl Pts',(-16.025045951378,8.28324661243913,8.));
#14925=CARTESIAN_POINT('Ctrl Pts',(-16.0839845137402,8.32890401789326,8.));
#14926=CARTESIAN_POINT('Ctrl Pts',(-16.1402813323094,8.37762295878361,8.));
#14927=CARTESIAN_POINT('Ctrl Pts',(-16.1798064165517,8.41182773787818,8.));
#14928=CARTESIAN_POINT('Ctrl Pts',(-16.2180286078769,8.4475424782692,8.));
#14929=CARTESIAN_POINT('Ctrl Pts',(-16.2548524753579,8.48468236692164,8.));
#14930=CARTESIAN_POINT('Ctrl Pts',(-16.2688611594934,8.4988112731053,8.));
#14931=CARTESIAN_POINT('Ctrl Pts',(-16.2826673549471,8.5131464868812,8.));
#14932=CARTESIAN_POINT('Ctrl Pts',(-16.2962653477309,8.52768352141437,8.));
#14933=CARTESIAN_POINT('Ctrl Pts',(-16.3091902201709,8.54150095167668,8.));
#14934=CARTESIAN_POINT('Ctrl Pts',(-16.3219308141586,8.55550525640342,8.));
#14935=CARTESIAN_POINT('Ctrl Pts',(-16.3344602231157,8.56966738394869,8.));
#14936=CARTESIAN_POINT('Ctrl Pts',(-16.3825593087518,8.62403430484007,8.));
#14937=CARTESIAN_POINT('Ctrl Pts',(-16.4276039578114,8.68077946858957,8.));
#14938=CARTESIAN_POINT('Ctrl Pts',(-16.4693716176289,8.73965492650984,8.));
#14939=CARTESIAN_POINT('Ctrl Pts',(-16.5102413746783,8.79726470574788,8.));
#14940=CARTESIAN_POINT('Ctrl Pts',(-16.5479738782328,8.85691503747699,8.));
#14941=CARTESIAN_POINT('Ctrl Pts',(-16.5823154929831,8.91839275710173,8.));
#14942=CARTESIAN_POINT('Ctrl Pts',(-16.6159043360375,8.97852287884562,8.));
#14943=CARTESIAN_POINT('Ctrl Pts',(-16.6462495962695,9.04040187061098,8.));
#14944=CARTESIAN_POINT('Ctrl Pts',(-16.6730657146258,9.10383727944419,8.));
#14945=CARTESIAN_POINT('Ctrl Pts',(-16.6817773057965,9.12444515938257,8.));
#14946=CARTESIAN_POINT('Ctrl Pts',(-16.6901160396164,9.14521730998075,8.));
#14947=CARTESIAN_POINT('Ctrl Pts',(-16.6980709212983,9.1661471082209,8.));
#14948=CARTESIAN_POINT('Ctrl Pts',(-16.7025653313911,9.17797218623112,8.));
#14949=CARTESIAN_POINT('Ctrl Pts',(-16.7069375536196,9.18984887021962,8.));
#14950=CARTESIAN_POINT('Ctrl Pts',(-16.711179782049,9.20175897829843,8.));
#14951=CARTESIAN_POINT('Ctrl Pts',(-16.734096120241,9.26609687739624,8.));
#14952=CARTESIAN_POINT('Ctrl Pts',(-16.7532666512879,9.33152043561446,8.));
#14953=CARTESIAN_POINT('Ctrl Pts',(-16.7684630804155,9.39783015254818,8.));
#14954=CARTESIAN_POINT('Ctrl Pts',(-16.770660460792,9.40741843605486,8.));
#14955=CARTESIAN_POINT('Ctrl Pts',(-16.7727746597823,9.41702526171543,8.));
#14956=CARTESIAN_POINT('Ctrl Pts',(-16.7748048961907,9.42665003738271,8.));
#14957=CARTESIAN_POINT('Ctrl Pts',(-16.7891235197531,9.49453057537518,8.));
#14958=CARTESIAN_POINT('Ctrl Pts',(-16.7992700679188,9.56330447632077,8.));
#14959=CARTESIAN_POINT('Ctrl Pts',(-16.8053412035889,9.63261589594071,8.));
#14960=CARTESIAN_POINT('Ctrl Pts',(-16.8110052242317,9.69727946678601,8.));
#14961=CARTESIAN_POINT('Ctrl Pts',(-16.813121294483,9.76241159112694,8.));
#14962=CARTESIAN_POINT('Ctrl Pts',(-16.8117297557015,9.82771097976151,8.));
#14963=CARTESIAN_POINT('Ctrl Pts',(-16.8114209501081,9.84220199986072,8.));
#14964=CARTESIAN_POINT('Ctrl Pts',(-16.8109392718932,9.85670118401844,8.));
#14965=CARTESIAN_POINT('Ctrl Pts',(-16.8102849391738,9.87120509964638,8.));
#14966=CARTESIAN_POINT('Ctrl Pts',(-16.8097777153087,9.88244820567933,8.));
#14967=CARTESIAN_POINT('Ctrl Pts',(-16.8091667038368,9.89369326677607,8.));
#14968=CARTESIAN_POINT('Ctrl Pts',(-16.8084530650648,9.90492595177548,8.));
#14969=CARTESIAN_POINT('Ctrl Pts',(-16.8041173130474,9.97317075371321,8.));
#14970=CARTESIAN_POINT('Ctrl Pts',(-16.7959925101146,10.0410849030563,8.));
#14971=CARTESIAN_POINT('Ctrl Pts',(-16.7841889169068,10.1083325876079,8.));
#14972=CARTESIAN_POINT('Ctrl Pts',(-16.772440263585,10.1752672674618,8.));
#14973=CARTESIAN_POINT('Ctrl Pts',(-16.7570464996027,10.2415426993447,8.));
#14974=CARTESIAN_POINT('Ctrl Pts',(-16.7380692198235,10.3068079361699,8.));
#14975=CARTESIAN_POINT('Ctrl Pts',(-16.7194994223666,10.3706717903636,8.));
#14976=CARTESIAN_POINT('Ctrl Pts',(-16.6974978125829,10.4335691780139,8.));
#14977=CARTESIAN_POINT('Ctrl Pts',(-16.6720845678673,10.4951388738486,8.));
#14978=CARTESIAN_POINT('Ctrl Pts',(-16.6666982087073,10.5081886240417,8.));
#14979=CARTESIAN_POINT('Ctrl Pts',(-16.6611584673709,10.5211785874357,8.));
#14980=CARTESIAN_POINT('Ctrl Pts',(-16.6554653473059,10.5341050800545,8.));
#14981=CARTESIAN_POINT('Ctrl Pts',(-16.6501415194561,10.5461930776059,8.));
#14982=CARTESIAN_POINT('Ctrl Pts',(-16.6446827914777,10.5582269434921,8.));
#14983=CARTESIAN_POINT('Ctrl Pts',(-16.6390983290274,10.5701847169649,8.));
#14984=CARTESIAN_POINT('Ctrl Pts',(-16.6114456278208,10.6293962775905,8.));
#14985=CARTESIAN_POINT('Ctrl Pts',(-16.5806669622525,10.6868526416772,8.));
#14986=CARTESIAN_POINT('Ctrl Pts',(-16.5468263628228,10.7422402982346,8.));
#14987=CARTESIAN_POINT('Ctrl Pts',(-16.5136306620755,10.796572434874,8.));
#14988=CARTESIAN_POINT('Ctrl Pts',(-16.4774881013739,10.8489146747283,8.));
#14989=CARTESIAN_POINT('Ctrl Pts',(-16.438424559325,10.8989353653364,8.));
#14990=CARTESIAN_POINT('Ctrl Pts',(-16.4006315217879,10.9473291806082,8.));
#14991=CARTESIAN_POINT('Ctrl Pts',(-16.360103934621,10.9935504630778,8.));
#14992=CARTESIAN_POINT('Ctrl Pts',(-16.316839891742,11.0372567981819,8.));
#14993=CARTESIAN_POINT('Ctrl Pts',(-16.3096319230205,11.0445384546198,8.));
#14994=CARTESIAN_POINT('Ctrl Pts',(-16.3023479491257,11.0517501974988,8.));
#14995=CARTESIAN_POINT('Ctrl Pts',(-16.2949879039586,11.0588903115368,8.));
#14996=CARTESIAN_POINT('Ctrl Pts',(-16.2872272673507,11.0664190466369,8.));
#14997=CARTESIAN_POINT('Ctrl Pts',(-16.2793820521969,11.0738681429984,8.));
#14998=CARTESIAN_POINT('Ctrl Pts',(-16.271453753893,11.081236856086,8.));
#14999=CARTESIAN_POINT('Origin',(15.,-10.,9.54592528053767));
#15000=CARTESIAN_POINT('Ctrl Pts',(12.9434529369556,-9.99851181185547,7.79592528053768));
#15001=CARTESIAN_POINT('Ctrl Pts',(12.9426313731505,-9.9001452310185,7.79057696270225));
#15002=CARTESIAN_POINT('Ctrl Pts',(12.9937603976267,-9.12123426690962,7.74818159569048));
#15003=CARTESIAN_POINT('Ctrl Pts',(13.9893910509183,-7.79139173496881,7.66873917950237));
#15004=CARTESIAN_POINT('Ctrl Pts',(16.3073489540956,-7.95337086724347,7.55759803197335));
#15005=CARTESIAN_POINT('Ctrl Pts',(17.4286195209518,-9.9883529914062,7.44645688444433));
#15006=CARTESIAN_POINT('Ctrl Pts',(16.3268235646033,-12.0342028814299,7.33531573691532));
#15007=CARTESIAN_POINT('Ctrl Pts',(14.0105079567266,-12.2179173173397,7.22417458938628));
#15008=CARTESIAN_POINT('Ctrl Pts',(12.9977472715797,-10.8922265383227,7.14437777059375));
#15009=CARTESIAN_POINT('Ctrl Pts',(12.9427343868833,-10.1065382000683,7.10162800097755));
#15010=CARTESIAN_POINT('Ctrl Pts',(12.9436342636416,-10.0016028715607,7.09592528053768));
#15011=CARTESIAN_POINT('Ctrl Pts',(12.9473113312417,-10.0024712008536,7.85407471946232));
#15012=CARTESIAN_POINT('Ctrl Pts',(12.950875636899,-9.53216658348607,7.82862238128887));
#15013=CARTESIAN_POINT('Ctrl Pts',(13.3435593652589,-8.37020036788621,7.76612299393908));
#15014=CARTESIAN_POINT('Ctrl Pts',(15.2723376840439,-7.58731246609672,7.66657655741293));
#15015=CARTESIAN_POINT('Ctrl Pts',(17.1748664515305,-8.91924865455582,7.55543540988393));
#15016=CARTESIAN_POINT('Ctrl Pts',(17.0874396573092,-11.2417232863365,7.44429426235489));
#15017=CARTESIAN_POINT('Ctrl Pts',(15.0888244971834,-12.4269237058338,7.33315311482589));
#15018=CARTESIAN_POINT('Ctrl Pts',(13.2786047494337,-11.5251874796858,7.23641326719502));
#15019=CARTESIAN_POINT('Ctrl Pts',(12.9501054372198,-10.417780757041,7.1767204687405));
#15020=CARTESIAN_POINT('Ctrl Pts',(12.9479406426496,-9.99884121834684,7.15407471946232));
#15021=CARTESIAN_POINT('Ctrl Pts',(16.2690708798524,-8.92064134695149,8.));
#15022=CARTESIAN_POINT('Ctrl Pts',(16.6279938291456,-9.34264997380806,7.96295295082366));
#15023=CARTESIAN_POINT('Ctrl Pts',(16.8854605771123,-10.5656667587716,7.88885885247099));
#15024=CARTESIAN_POINT('Ctrl Pts',(15.5448841833265,-11.8935743297638,7.77771770494195));
#15025=CARTESIAN_POINT('Ctrl Pts',(13.705710965359,-11.4833634608872,7.66657655741295));
#15026=CARTESIAN_POINT('Ctrl Pts',(13.0512228097228,-9.71772794909045,7.55543540988392));
#15027=CARTESIAN_POINT('Ctrl Pts',(14.1805939850735,-8.20925106726273,7.44429426235491));
#15028=CARTESIAN_POINT('Ctrl Pts',(16.0600040674161,-8.34058443354548,7.33315311482588));
#15029=CARTESIAN_POINT('Ctrl Pts',(16.9691349905856,-9.99055655611766,7.22201196729687));
#15030=CARTESIAN_POINT('Ctrl Pts',(16.075794164073,-11.649340309265,7.11087081976784));
#15031=CARTESIAN_POINT('Ctrl Pts',(14.1977156617139,-11.7982967517645,6.99972967223883));
#15032=CARTESIAN_POINT('Ctrl Pts',(13.0540156107808,-10.3012080182464,6.88858852470979));
#15033=CARTESIAN_POINT('Ctrl Pts',(13.6915932046182,-8.52838237790974,6.77744737718079));
#15034=CARTESIAN_POINT('Ctrl Pts',(15.5268344070607,-8.10262919057289,6.66630622965176));
#15035=CARTESIAN_POINT('Ctrl Pts',(16.8798323474503,-9.41364810779719,6.55516508212274));
#15036=CARTESIAN_POINT('Ctrl Pts',(16.5121060130156,-11.2613935227057,6.44402393459372));
#15037=CARTESIAN_POINT('Ctrl Pts',(14.7602576499653,-11.9545075482124,6.33288278706471));
#15038=CARTESIAN_POINT('Ctrl Pts',(13.2278599385176,-10.8585434774938,6.22174163953568));
#15039=CARTESIAN_POINT('Ctrl Pts',(13.3176091852349,-8.97670221714518,6.11060049200667));
#15040=CARTESIAN_POINT('Ctrl Pts',(14.9473524645216,-8.03154751397968,5.99945934447764));
#15041=CARTESIAN_POINT('Ctrl Pts',(16.6252872186854,-8.88823627676186,5.88831819694863));
#15042=CARTESIAN_POINT('Ctrl Pts',(16.8154983086942,-10.7625896568447,5.7771770494196));
#15043=CARTESIAN_POINT('Ctrl Pts',(15.3438740247519,-11.9388985839416,5.66603590189059));
#15044=CARTESIAN_POINT('Ctrl Pts',(13.5574810535658,-11.3404164190708,5.55489475436156));
#15045=CARTESIAN_POINT('Ctrl Pts',(13.091512894956,-9.51497005045939,5.44375360683255));
#15046=CARTESIAN_POINT('Ctrl Pts',(14.3724983786311,-8.13350092582179,5.33261245930352));
#15047=CARTESIAN_POINT('Ctrl Pts',(16.2278740377661,-8.46055125795619,5.22147131177451));
#15048=CARTESIAN_POINT('Ctrl Pts',(16.9593023477033,-10.1967521063248,5.11033016424548));
#15049=CARTESIAN_POINT('Ctrl Pts',(15.8972627511728,-11.7528538547388,4.99918901671647));
#15050=CARTESIAN_POINT('Ctrl Pts',(14.0139043062234,-11.7044624853229,4.88804786918744));
#15051=CARTESIAN_POINT('Ctrl Pts',(13.0331788732669,-10.0958735439955,4.77690672165843));
#15052=CARTESIAN_POINT('Ctrl Pts',(13.8528037398514,-8.39952575101248,4.66576557412941));
#15053=CARTESIAN_POINT('Ctrl Pts',(15.7225267076418,-8.16818880946363,4.55462442660038));
#15054=CARTESIAN_POINT('Ctrl Pts',(16.930877292936,-9.61361940961134,4.44348327907137));
#15055=CARTESIAN_POINT('Ctrl Pts',(16.3717791430773,-11.4127275263198,4.33234213154234));
#15056=CARTESIAN_POINT('Ctrl Pts',(14.5570086000468,-11.9186807187697,4.22120098401333));
#15057=CARTESIAN_POINT('Ctrl Pts',(13.1477348705092,-10.6683494378538,4.1100598364843));
#15058=CARTESIAN_POINT('Ctrl Pts',(13.4339514097027,-8.80623750526538,3.99891868895529));
#15059=CARTESIAN_POINT('Ctrl Pts',(15.1536669134528,-8.03684856398734,3.88777754142627));
#15060=CARTESIAN_POINT('Ctrl Pts',(16.7327217999743,-9.0644508324513,3.77663639389725));
#15061=CARTESIAN_POINT('Ctrl Pts',(16.7257116553616,-10.948417821193,3.66549524636823));
#15062=CARTESIAN_POINT('Ctrl Pts',(15.139053288841,-11.9642406328842,3.55435409883921));
#15063=CARTESIAN_POINT('Ctrl Pts',(13.4251110393005,-11.1820752270774,3.44321295131019));
#15064=CARTESIAN_POINT('Ctrl Pts',(13.1527598798706,-9.31788489271265,3.33207180378117));
#15065=CARTESIAN_POINT('Ctrl Pts',(14.5712992942719,-8.07807575957374,3.22093065625215));
#15066=CARTESIAN_POINT('Ctrl Pts',(16.3822543856635,-8.59752009130784,3.10978950872313));
#15067=CARTESIAN_POINT('Ctrl Pts',(16.927948460973,-10.400739083237,2.9986483611941));
#15068=CARTESIAN_POINT('Ctrl Pts',(15.7088747381036,-11.8371373619946,2.88750721366509));
#15069=CARTESIAN_POINT('Ctrl Pts',(13.8409251059329,-11.5918927321457,2.77636606613606));
#15070=CARTESIAN_POINT('Ctrl Pts',(13.0339468067845,-9.88949243235736,2.66522491860705));
#15071=CARTESIAN_POINT('Ctrl Pts',(14.0266158712758,-8.28824639040892,2.55408377107803));
#15072=CARTESIAN_POINT('Ctrl Pts',(15.910282283518,-8.25387192822464,2.44294262354901));
#15073=CARTESIAN_POINT('Ctrl Pts',(16.960712282471,-9.8178340661976,2.33180147601999));
#15074=CARTESIAN_POINT('Ctrl Pts',(16.21638377583,-11.5485437020743,2.22066032849097));
#15075=CARTESIAN_POINT('Ctrl Pts',(14.3586256526202,-11.8617776479034,2.10951918096195));
#15076=CARTESIAN_POINT('Ctrl Pts',(13.0879562476019,-10.470813957433,1.99837803343293));
#15077=CARTESIAN_POINT('Ctrl Pts',(13.5674961034851,-8.64888575390523,1.88723688590391));
#15078=CARTESIAN_POINT('Ctrl Pts',(15.358293382976,-8.06371417284865,1.77609573837489));
#15079=CARTESIAN_POINT('Ctrl Pts',(16.8211230807301,-9.25094197098372,1.66495459084587));
#15080=CARTESIAN_POINT('Ctrl Pts',(16.6169686796854,-11.1238280959179,1.55381344331685));
#15081=CARTESIAN_POINT('Ctrl Pts',(14.9327051361131,-11.9680059836581,1.44267229578783));
#15082=CARTESIAN_POINT('Ctrl Pts',(13.3100405366278,-11.0107498334803,1.33153114825881));
#15083=CARTESIAN_POINT('Ctrl Pts',(13.234298236499,-9.12829163226479,1.22039000072979));
#15084=CARTESIAN_POINT('Ctrl Pts',(14.7748090948109,-8.04376393624155,1.10924885320077));
#15085=CARTESIAN_POINT('Ctrl Pts',(16.5214516331146,-8.74989132634765,0.998107705671752));
#15086=CARTESIAN_POINT('Ctrl Pts',(16.875415892384,-10.6003305289044,0.886966558142729));
#15087=CARTESIAN_POINT('Ctrl Pts',(15.5127017026779,-11.9012281112315,0.775825410613712));
#15088=CARTESIAN_POINT('Ctrl Pts',(13.6806746106472,-11.4618608197188,0.66468426308469));
#15089=CARTESIAN_POINT('Ctrl Pts',(13.0563175150209,-9.68427830710207,0.553543115555672));
#15090=CARTESIAN_POINT('Ctrl Pts',(14.2111078511261,-8.19586091928163,0.442401968026651));
#15091=CARTESIAN_POINT('Ctrl Pts',(16.0880628102433,-8.35855938932811,0.331260820497632));
#15092=CARTESIAN_POINT('Ctrl Pts',(16.9689629508152,-10.0243915228465,0.220119672968611));
#15093=CARTESIAN_POINT('Ctrl Pts',(16.0477169744579,-11.6666854543434,0.108978525439592));
#15094=CARTESIAN_POINT('Ctrl Pts',(14.1671160606488,-11.7857286633614,-0.00216262208942931));
#15095=CARTESIAN_POINT('Ctrl Pts',(13.0494868752983,-10.2654035044801,-0.113303769618448));
#15096=CARTESIAN_POINT('Ctrl Pts',(13.4941166421103,-9.09734376582132,-0.187397867971128));
#15097=CARTESIAN_POINT('Ctrl Pts',(13.9143317362933,-8.73632265938643,-0.224444917147468));
#15098=CARTESIAN_POINT('Ctrl Pts',(16.3677806246588,-8.83668763019027,8.07481497238249));
#15099=CARTESIAN_POINT('Ctrl Pts',(16.7546210002301,-9.29152055750512,8.03776792320615));
#15100=CARTESIAN_POINT('Ctrl Pts',(17.0321137982713,-10.609664948542,7.96367382485346));
#15101=CARTESIAN_POINT('Ctrl Pts',(15.5872658812593,-12.04085864763,7.85253267732446));
#15102=CARTESIAN_POINT('Ctrl Pts',(13.6050397244193,-11.5987411210352,7.74139152979541));
#15103=CARTESIAN_POINT('Ctrl Pts',(12.8996447519557,-9.69577251495858,7.63025038226642));
#15104=CARTESIAN_POINT('Ctrl Pts',(14.1168596736884,-8.06996462316475,7.51910923473738));
#15105=CARTESIAN_POINT('Ctrl Pts',(16.142452362976,-8.21151324477814,7.40796808720838));
#15106=CARTESIAN_POINT('Ctrl Pts',(17.1222965007077,-9.98982203454717,7.29682693967935));
#15107=CARTESIAN_POINT('Ctrl Pts',(16.1594706309165,-11.77762783332,7.18568579215033));
#15108=CARTESIAN_POINT('Ctrl Pts',(14.1353130933848,-11.9381702736228,7.07454464462131));
#15109=CARTESIAN_POINT('Ctrl Pts',(12.9026547801867,-10.324636312983,6.9634034970923));
#15110=CARTESIAN_POINT('Ctrl Pts',(13.5898238685428,-8.41391832216992,6.85226234956327));
#15111=CARTESIAN_POINT('Ctrl Pts',(15.5678121733162,-7.95504957829503,6.74112120203425));
#15112=CARTESIAN_POINT('Ctrl Pts',(17.026047798645,-9.36804100533744,6.62998005450523));
#15113=CARTESIAN_POINT('Ctrl Pts',(16.6297193008426,-11.3595061141326,6.51883890697621));
#15114=CARTESIAN_POINT('Ctrl Pts',(14.7416102232794,-12.1065313195945,6.4076977594472));
#15115=CARTESIAN_POINT('Ctrl Pts',(13.0900209131272,-10.9253219442557,6.29655661191817));
#15116=CARTESIAN_POINT('Ctrl Pts',(13.1867509560953,-8.89710897723226,6.18541546438916));
#15117=CARTESIAN_POINT('Ctrl Pts',(14.9432574806446,-7.87843908982193,6.07427431686013));
#15118=CARTESIAN_POINT('Ctrl Pts',(16.7517038665974,-8.80176205759242,5.96313316933111));
#15119=CARTESIAN_POINT('Ctrl Pts',(16.9567097867864,-10.8219047286931,5.8519920218021));
#15120=CARTESIAN_POINT('Ctrl Pts',(15.3706209289381,-12.0897082727185,5.74085087427307));
#15121=CARTESIAN_POINT('Ctrl Pts',(13.4452803251892,-11.4446754992856,5.62970972674406));
#15122=CARTESIAN_POINT('Ctrl Pts',(12.9430686448388,-9.47724388141499,5.51856857921503));
#15123=CARTESIAN_POINT('Ctrl Pts',(14.3236906044599,-7.98832255145469,5.40742743168601));
#15124=CARTESIAN_POINT('Ctrl Pts',(16.3233794463658,-8.340811222248,5.29628628415699));
#15125=CARTESIAN_POINT('Ctrl Pts',(17.1116990639237,-10.2120557040307,5.18514513662797));
#15126=CARTESIAN_POINT('Ctrl Pts',(15.9670528461145,-11.8891927775139,5.07400398909896));
#15127=CARTESIAN_POINT('Ctrl Pts',(13.9372046861842,-11.8370374735521,4.96286284156993));
#15128=CARTESIAN_POINT('Ctrl Pts',(12.8801973380494,-10.1033306949015,4.85172169404091));
#15129=CARTESIAN_POINT('Ctrl Pts',(13.7635735385443,-8.27503908348669,4.74058054651189));
#15130=CARTESIAN_POINT('Ctrl Pts',(15.7787256387334,-8.02570849727455,4.62943939898287));
#15131=CARTESIAN_POINT('Ctrl Pts',(17.0810630767753,-9.58356629746378,4.51829825145386));
#15132=CARTESIAN_POINT('Ctrl Pts',(16.4784776508547,-11.5226110448986,4.40715710392483));
#15133=CARTESIAN_POINT('Ctrl Pts',(14.5225522361549,-12.0679178395023,4.29601595639582));
#15134=CARTESIAN_POINT('Ctrl Pts',(13.0036636281943,-10.720334400632,4.18487480886679));
#15135=CARTESIAN_POINT('Ctrl Pts',(13.3121424082065,-8.71338533042983,4.07373366133778));
#15136=CARTESIAN_POINT('Ctrl Pts',(15.1656192969272,-7.88415246139632,3.96259251380876));
#15137=CARTESIAN_POINT('Ctrl Pts',(16.8674948291339,-8.99168277745238,3.85145136627974));
#15138=CARTESIAN_POINT('Ctrl Pts',(16.8599394276748,-11.022186814388,3.74031021875072));
#15139=CARTESIAN_POINT('Ctrl Pts',(15.1498690083362,-12.1170214544196,3.62916907122169));
#15140=CARTESIAN_POINT('Ctrl Pts',(13.3026144239599,-11.2740183532331,3.51802792369268));
#15141=CARTESIAN_POINT('Ctrl Pts',(13.009079488374,-9.26482922085231,3.40688677616365));
#15142=CARTESIAN_POINT('Ctrl Pts',(14.5379544764744,-7.92858635411841,3.29574562863464));
#15143=CARTESIAN_POINT('Ctrl Pts',(16.4897676694624,-8.48843364382804,3.18460448110562));
#15144=CARTESIAN_POINT('Ctrl Pts',(17.077906437004,-10.4319090149314,3.0734633335766));
#15145=CARTESIAN_POINT('Ctrl Pts',(15.7640118038174,-11.9800319497248,2.96232218604758));
#15146=CARTESIAN_POINT('Ctrl Pts',(13.7507709712654,-11.7157119197451,2.85118103851856));
#15147=CARTESIAN_POINT('Ctrl Pts',(12.8810250022902,-9.88089703081255,2.74003989098954));
#15148=CARTESIAN_POINT('Ctrl Pts',(13.9509049709074,-8.15510429042321,2.62889874346052));
#15149=CARTESIAN_POINT('Ctrl Pts',(15.981085052169,-8.11805614433055,2.5177575959315));
#15150=CARTESIAN_POINT('Ctrl Pts',(17.1132186649861,-9.80366499721687,2.40661644840248));
#15151=CARTESIAN_POINT('Ctrl Pts',(16.310995459074,-11.6689911538913,2.29547530087346));
#15152=CARTESIAN_POINT('Ctrl Pts',(14.3087388423873,-12.0065887844825,2.18433415334444));
#15153=CARTESIAN_POINT('Ctrl Pts',(12.9392353574969,-10.5074343907968,2.07319300581542));
#15154=CARTESIAN_POINT('Ctrl Pts',(13.4560743568324,-8.54379458480371,1.9620518582864));
#15155=CARTESIAN_POINT('Ctrl Pts',(15.3861618408855,-7.91310770720139,1.85091071075738));
#15156=CARTESIAN_POINT('Ctrl Pts',(16.9627720598485,-9.19267940420098,1.73976956322836));
#15157=CARTESIAN_POINT('Ctrl Pts',(16.74273830238,-11.2112406954153,1.62862841569934));
#15158=CARTESIAN_POINT('Ctrl Pts',(14.9274708667381,-12.1210796783654,1.51748726817032));
#15159=CARTESIAN_POINT('Ctrl Pts',(13.1785936095798,-11.0893670799319,1.4063461206413));
#15160=CARTESIAN_POINT('Ctrl Pts',(13.0969599890878,-9.06048918569476,1.29520497311228));
#15161=CARTESIAN_POINT('Ctrl Pts',(14.7572934956928,-7.89160571899742,1.18406382558326));
#15162=CARTESIAN_POINT('Ctrl Pts',(16.6397918336695,-8.65265648303387,1.07292267805424));
#15163=CARTESIAN_POINT('Ctrl Pts',(17.0212878267906,-10.6470249052772,0.961781530525217));
#15164=CARTESIAN_POINT('Ctrl Pts',(15.5525802114646,-12.0491077487348,0.850640382996201));
#15165=CARTESIAN_POINT('Ctrl Pts',(13.5780560141864,-11.5755659805163,0.739499235467179));
#15166=CARTESIAN_POINT('Ctrl Pts',(12.9051357290994,-9.65972112260545,0.628358087938161));
#15167=CARTESIAN_POINT('Ctrl Pts',(14.1497469421876,-8.0555329745779,0.51721694040914));
#15168=CARTESIAN_POINT('Ctrl Pts',(16.172693546034,-8.23088631261769,0.406075792880121));
#15169=CARTESIAN_POINT('Ctrl Pts',(17.1221110794925,-10.0262887226278,0.2949346453511));
#15170=CARTESIAN_POINT('Ctrl Pts',(16.1292095662587,-11.796322103078,0.18379349782208));
#15171=CARTESIAN_POINT('Ctrl Pts',(14.1023334213085,-11.9246246253225,0.0726523502930598));
#15172=CARTESIAN_POINT('Ctrl Pts',(12.8977737946205,-10.2860468843054,-0.0384887972359588));
#15173=CARTESIAN_POINT('Ctrl Pts',(13.3769873593213,-9.02713415977151,-0.112582895588639));
#15174=CARTESIAN_POINT('Ctrl Pts',(13.829887250996,-8.638032430062,-0.149629944764979));
#15175=CARTESIAN_POINT('Ctrl Pts',(16.4664903694653,-8.75273391342904,8.14962994476498));
#15176=CARTESIAN_POINT('Ctrl Pts',(16.8812481713146,-9.24039114120218,8.11258289558864));
#15177=CARTESIAN_POINT('Ctrl Pts',(17.1787670194302,-10.6536631383124,8.03848879723595));
#15178=CARTESIAN_POINT('Ctrl Pts',(15.6296475791921,-12.1881429654964,7.92734764970695));
#15179=CARTESIAN_POINT('Ctrl Pts',(13.5043684834796,-11.7141187811832,7.81620650217791));
#15180=CARTESIAN_POINT('Ctrl Pts',(12.7480666941885,-9.67381708082673,7.7050653546489));
#15181=CARTESIAN_POINT('Ctrl Pts',(14.0531253623034,-7.93067817906678,7.59392420711987));
#15182=CARTESIAN_POINT('Ctrl Pts',(16.2249006585358,-8.08244205601081,7.48278305959086));
#15183=CARTESIAN_POINT('Ctrl Pts',(17.2754580108298,-9.98908751297668,7.37164191206184));
#15184=CARTESIAN_POINT('Ctrl Pts',(16.2431470977599,-11.9059153573749,7.26050076453283));
#15185=CARTESIAN_POINT('Ctrl Pts',(14.0729105250557,-12.0780437954813,7.1493596170038));
#15186=CARTESIAN_POINT('Ctrl Pts',(12.7512939495927,-10.3480646077196,7.03821846947479));
#15187=CARTESIAN_POINT('Ctrl Pts',(13.4880545324674,-8.2994542664301,6.92707732194575));
#15188=CARTESIAN_POINT('Ctrl Pts',(15.6087899395717,-7.80746996601717,6.81593617441675));
#15189=CARTESIAN_POINT('Ctrl Pts',(17.1722632498397,-9.32243390287767,6.70479502688772));
#15190=CARTESIAN_POINT('Ctrl Pts',(16.7473325886698,-11.4576187055596,6.5936538793587));
#15191=CARTESIAN_POINT('Ctrl Pts',(14.7229627965935,-12.2585550909766,6.48251273182968));
#15192=CARTESIAN_POINT('Ctrl Pts',(12.9521818877368,-10.9921004110175,6.37137158430066));
#15193=CARTESIAN_POINT('Ctrl Pts',(13.0558927269556,-8.81751573731931,6.26023043677165));
#15194=CARTESIAN_POINT('Ctrl Pts',(14.9391624967676,-7.72533066566421,6.14908928924262));
#15195=CARTESIAN_POINT('Ctrl Pts',(16.8781205145093,-8.71528783842296,6.0379481417136));
#15196=CARTESIAN_POINT('Ctrl Pts',(17.0979212648787,-10.8812198005416,5.92680699418458));
#15197=CARTESIAN_POINT('Ctrl Pts',(15.3973678331242,-12.2405179614955,5.81566584665556));
#15198=CARTESIAN_POINT('Ctrl Pts',(13.3330795968126,-11.5489345795005,5.70452469912655));
#15199=CARTESIAN_POINT('Ctrl Pts',(12.7946243947216,-9.43951771237056,5.59338355159752));
#15200=CARTESIAN_POINT('Ctrl Pts',(14.2748828302889,-7.8431441770876,5.48224240406851));
#15201=CARTESIAN_POINT('Ctrl Pts',(16.4188848549655,-8.2210711865398,5.37110125653948));
#15202=CARTESIAN_POINT('Ctrl Pts',(17.2640957801442,-10.2273593017365,5.25996010901047));
#15203=CARTESIAN_POINT('Ctrl Pts',(16.0368429410561,-12.025531700289,5.14881896148144));
#15204=CARTESIAN_POINT('Ctrl Pts',(13.8605050661451,-11.9696124617812,5.03767781395242));
#15205=CARTESIAN_POINT('Ctrl Pts',(12.7272158028318,-10.1107878458076,4.9265366664234));
#15206=CARTESIAN_POINT('Ctrl Pts',(13.6743433372372,-8.15055241596089,4.81539551889439));
#15207=CARTESIAN_POINT('Ctrl Pts',(15.8349245698249,-7.88322818508548,4.70425437136536));
#15208=CARTESIAN_POINT('Ctrl Pts',(17.2312488606147,-9.55351318531619,4.59311322383635));
#15209=CARTESIAN_POINT('Ctrl Pts',(16.585176158632,-11.6324945634774,4.48197207630732));
#15210=CARTESIAN_POINT('Ctrl Pts',(14.488095872263,-12.2171549602349,4.37083092877831));
#15211=CARTESIAN_POINT('Ctrl Pts',(12.8595923858795,-10.7723193634102,4.25968978124928));
#15212=CARTESIAN_POINT('Ctrl Pts',(13.1903334067103,-8.62053315559428,4.14854863372026));
#15213=CARTESIAN_POINT('Ctrl Pts',(15.1775716804015,-7.7314563588053,4.03740748619125));
#15214=CARTESIAN_POINT('Ctrl Pts',(17.0022678582936,-8.91891472245348,3.92626633866222));
#15215=CARTESIAN_POINT('Ctrl Pts',(16.9941671999881,-11.0959558075831,3.81512519113321));
#15216=CARTESIAN_POINT('Ctrl Pts',(15.1606847278314,-12.269802275955,3.70398404360418));
#15217=CARTESIAN_POINT('Ctrl Pts',(13.1801178086194,-11.3659614793888,3.59284289607517));
#15218=CARTESIAN_POINT('Ctrl Pts',(12.8653990968773,-9.21177354899199,3.48170174854614));
#15219=CARTESIAN_POINT('Ctrl Pts',(14.5046096586769,-7.77909694866307,3.37056060101713));
#15220=CARTESIAN_POINT('Ctrl Pts',(16.5972809532612,-8.37934719634824,3.25941945348811));
#15221=CARTESIAN_POINT('Ctrl Pts',(17.2278644130351,-10.4630789466257,3.14827830595909));
#15222=CARTESIAN_POINT('Ctrl Pts',(15.8191488695313,-12.122926537455,3.03713715843007));
#15223=CARTESIAN_POINT('Ctrl Pts',(13.6606168365978,-11.8395311073445,2.92599601090104));
#15224=CARTESIAN_POINT('Ctrl Pts',(12.7281031977959,-9.87230162926771,2.81485486337203));
#15225=CARTESIAN_POINT('Ctrl Pts',(13.8751940705389,-8.02196219043751,2.70371371584301));
#15226=CARTESIAN_POINT('Ctrl Pts',(16.05188782082,-7.98224036043646,2.59257256831398));
#15227=CARTESIAN_POINT('Ctrl Pts',(17.2657250475012,-9.78949592823614,2.48143142078497));
#15228=CARTESIAN_POINT('Ctrl Pts',(16.4056071423181,-11.7894386057083,2.37029027325595));
#15229=CARTESIAN_POINT('Ctrl Pts',(14.2588520321544,-12.1513999210617,2.25914912572693));
#15230=CARTESIAN_POINT('Ctrl Pts',(12.790514467392,-10.5440548241605,2.14800797819791));
#15231=CARTESIAN_POINT('Ctrl Pts',(13.3446526101798,-8.43870341570221,2.03686683066888));
#15232=CARTESIAN_POINT('Ctrl Pts',(15.414030298795,-7.76250124155411,1.92572568313987));
#15233=CARTESIAN_POINT('Ctrl Pts',(17.1044210389669,-9.13441683741825,1.81458453561085));
#15234=CARTESIAN_POINT('Ctrl Pts',(16.8685079250746,-11.2986532949127,1.70344338808183));
#15235=CARTESIAN_POINT('Ctrl Pts',(14.9222365973632,-12.2741533730727,1.59230224055281));
#15236=CARTESIAN_POINT('Ctrl Pts',(13.0471466825318,-11.1679843263836,1.48116109302379));
#15237=CARTESIAN_POINT('Ctrl Pts',(12.9596217416766,-8.99268673912471,1.37001994549477));
#15238=CARTESIAN_POINT('Ctrl Pts',(14.7397778965747,-7.73944750175331,1.25887879796575));
#15239=CARTESIAN_POINT('Ctrl Pts',(16.7581320342244,-8.55542163972007,1.14773765043673));
#15240=CARTESIAN_POINT('Ctrl Pts',(17.1671597611972,-10.6937192816501,1.03659650290771));
#15241=CARTESIAN_POINT('Ctrl Pts',(15.5924587202513,-12.196987386238,0.925455355378689));
#15242=CARTESIAN_POINT('Ctrl Pts',(13.4754374177256,-11.6892711413137,0.814314207849668));
#15243=CARTESIAN_POINT('Ctrl Pts',(12.7539539431779,-9.63516393810883,0.70317306032065));
#15244=CARTESIAN_POINT('Ctrl Pts',(14.0883860332491,-7.91520502987416,0.592031912791629));
#15245=CARTESIAN_POINT('Ctrl Pts',(16.2573242818248,-8.10321323590726,0.48089076526261));
#15246=CARTESIAN_POINT('Ctrl Pts',(17.2752592081698,-10.028185922409,0.369749617733589));
#15247=CARTESIAN_POINT('Ctrl Pts',(16.2107021580595,-11.9259587518127,0.25860847020457));
#15248=CARTESIAN_POINT('Ctrl Pts',(14.0375507819682,-12.0635205872837,0.147467322675549));
#15249=CARTESIAN_POINT('Ctrl Pts',(12.7460607139427,-10.3066902641307,0.0363261751465303));
#15250=CARTESIAN_POINT('Ctrl Pts',(13.2598580765323,-8.9569245537217,-0.0377679232061503));
#15251=CARTESIAN_POINT('Ctrl Pts',(13.7454427656987,-8.53974220073757,-0.0748149723824902));
#15252=CARTESIAN_POINT('Ctrl Pts',(16.5652001142717,-8.66878019666782,8.22444491714747));
#15253=CARTESIAN_POINT('Ctrl Pts',(17.0078753423991,-9.18926172489923,8.18739786797113));
#15254=CARTESIAN_POINT('Ctrl Pts',(17.3254202405892,-10.6976613280828,8.11330376961845));
#15255=CARTESIAN_POINT('Ctrl Pts',(15.6720292771249,-12.3354272833626,8.00216262208942));
#15256=CARTESIAN_POINT('Ctrl Pts',(13.4036972425399,-11.8294964413313,7.89102147456041));
#15257=CARTESIAN_POINT('Ctrl Pts',(12.5964886364213,-9.65186164669486,7.77988032703138));
#15258=CARTESIAN_POINT('Ctrl Pts',(13.9893910509183,-7.79139173496881,7.66873917950237));
#15259=CARTESIAN_POINT('Ctrl Pts',(16.3073489540956,-7.95337086724347,7.55759803197335));
#15260=CARTESIAN_POINT('Ctrl Pts',(17.4286195209518,-9.9883529914062,7.44645688444433));
#15261=CARTESIAN_POINT('Ctrl Pts',(16.3268235646033,-12.0342028814299,7.33531573691532));
#15262=CARTESIAN_POINT('Ctrl Pts',(14.0105079567266,-12.2179173173397,7.22417458938628));
#15263=CARTESIAN_POINT('Ctrl Pts',(12.5999331189987,-10.3714929024561,7.11303344185728));
#15264=CARTESIAN_POINT('Ctrl Pts',(13.3862851963921,-8.1849902106903,7.00189229432825));
#15265=CARTESIAN_POINT('Ctrl Pts',(15.6497677058271,-7.65989035373928,6.89075114679923));
#15266=CARTESIAN_POINT('Ctrl Pts',(17.3184787010345,-9.27682680041793,6.77960999927021));
#15267=CARTESIAN_POINT('Ctrl Pts',(16.8649458764968,-11.5557312969865,6.66846885174119));
#15268=CARTESIAN_POINT('Ctrl Pts',(14.7043153699076,-12.4105788623587,6.55732770421217));
#15269=CARTESIAN_POINT('Ctrl Pts',(12.8143428623464,-11.0588788777794,6.44618655668315));
#15270=CARTESIAN_POINT('Ctrl Pts',(12.9250344978159,-8.7379224974064,6.33504540915414));
#15271=CARTESIAN_POINT('Ctrl Pts',(14.9350675128906,-7.57222224150645,6.2239042616251));
#15272=CARTESIAN_POINT('Ctrl Pts',(17.0045371624213,-8.62881361925355,6.1127631140961));
#15273=CARTESIAN_POINT('Ctrl Pts',(17.2391327429709,-10.94053487239,6.00162196656707));
#15274=CARTESIAN_POINT('Ctrl Pts',(15.4241147373104,-12.3913276502725,5.89048081903805));
#15275=CARTESIAN_POINT('Ctrl Pts',(13.2208788684359,-11.6531936597153,5.77933967150903));
#15276=CARTESIAN_POINT('Ctrl Pts',(12.6461801446044,-9.40179154332619,5.66819852398002));
#15277=CARTESIAN_POINT('Ctrl Pts',(14.2260750561177,-7.69796580272048,5.55705737645098));
#15278=CARTESIAN_POINT('Ctrl Pts',(16.5143902635653,-8.10133115083163,5.44591622892198));
#15279=CARTESIAN_POINT('Ctrl Pts',(17.4164924963646,-10.2426628994423,5.33477508139295));
#15280=CARTESIAN_POINT('Ctrl Pts',(16.1066330359978,-12.161870623064,5.22363393386394));
#15281=CARTESIAN_POINT('Ctrl Pts',(13.7838054461059,-12.1021874500104,5.1124927863349));
#15282=CARTESIAN_POINT('Ctrl Pts',(12.5742342676142,-10.1182449967136,5.0013516388059));
#15283=CARTESIAN_POINT('Ctrl Pts',(13.5851131359301,-8.02606574843509,4.89021049127687));
#15284=CARTESIAN_POINT('Ctrl Pts',(15.8911235009165,-7.74074787289641,4.77906934374785));
#15285=CARTESIAN_POINT('Ctrl Pts',(17.381434644454,-9.52346007316861,4.66792819621884));
#15286=CARTESIAN_POINT('Ctrl Pts',(16.6918746664094,-11.7423780820561,4.55678704868981));
#15287=CARTESIAN_POINT('Ctrl Pts',(14.453639508371,-12.3663920809676,4.4456459011608));
#15288=CARTESIAN_POINT('Ctrl Pts',(12.7155211435647,-10.8243043261885,4.33450475363177));
#15289=CARTESIAN_POINT('Ctrl Pts',(13.0685244052141,-8.52768098075873,4.22336360610276));
#15290=CARTESIAN_POINT('Ctrl Pts',(15.1895240638759,-7.57876025621427,4.11222245857373));
#15291=CARTESIAN_POINT('Ctrl Pts',(17.1370408874533,-8.84614666745458,4.00108131104471));
#15292=CARTESIAN_POINT('Ctrl Pts',(17.1283949723014,-11.1697248007781,3.8899401635157));
#15293=CARTESIAN_POINT('Ctrl Pts',(15.1715004473266,-12.4225830974903,3.77879901598667));
#15294=CARTESIAN_POINT('Ctrl Pts',(13.0576211932789,-11.4579046055446,3.66765786845765));
#15295=CARTESIAN_POINT('Ctrl Pts',(12.7217187053807,-9.15871787713164,3.55651672092864));
#15296=CARTESIAN_POINT('Ctrl Pts',(14.4712648408794,-7.62960754320777,3.44537557339961));
#15297=CARTESIAN_POINT('Ctrl Pts',(16.7047942370601,-8.27026074886842,3.3342344258706));
#15298=CARTESIAN_POINT('Ctrl Pts',(17.3778223890662,-10.4942488783201,3.22309327834157));
#15299=CARTESIAN_POINT('Ctrl Pts',(15.8742859352451,-12.2658211251852,3.11195213081256));
#15300=CARTESIAN_POINT('Ctrl Pts',(13.5704627019302,-11.9633502949438,3.00081098328354));
#15301=CARTESIAN_POINT('Ctrl Pts',(12.5751813933016,-9.86370622772288,2.88966983575451));
#15302=CARTESIAN_POINT('Ctrl Pts',(13.7994831701705,-7.88882009045181,2.7785286882255));
#15303=CARTESIAN_POINT('Ctrl Pts',(16.122690589471,-7.84642457654237,2.66738754069648));
#15304=CARTESIAN_POINT('Ctrl Pts',(17.4182314300163,-9.77532685925541,2.55624639316745));
#15305=CARTESIAN_POINT('Ctrl Pts',(16.5002188255622,-11.9098860575253,2.44510524563844));
#15306=CARTESIAN_POINT('Ctrl Pts',(14.2089652219215,-12.2962110576408,2.33396409810941));
#15307=CARTESIAN_POINT('Ctrl Pts',(12.641793577287,-10.5806752575243,2.2228229505804));
#15308=CARTESIAN_POINT('Ctrl Pts',(13.2332308635271,-8.3336122466007,2.11168180305138));
#15309=CARTESIAN_POINT('Ctrl Pts',(15.4418987567046,-7.61189477590683,2.00054065552236));
#15310=CARTESIAN_POINT('Ctrl Pts',(17.2460700180853,-9.07615427063553,1.88939950799333));
#15311=CARTESIAN_POINT('Ctrl Pts',(16.9942775477693,-11.3860658944101,1.77825836046432));
#15312=CARTESIAN_POINT('Ctrl Pts',(14.9170023279882,-12.42722706778,1.6671172129353));
#15313=CARTESIAN_POINT('Ctrl Pts',(12.9156997554838,-11.2466015728353,1.55597606540628));
#15314=CARTESIAN_POINT('Ctrl Pts',(12.8222834942654,-8.92488429255467,1.44483491787726));
#15315=CARTESIAN_POINT('Ctrl Pts',(14.7222622974566,-7.58728928450919,1.33369377034824));
#15316=CARTESIAN_POINT('Ctrl Pts',(16.8764722347793,-8.45818679640628,1.22255262281922));
#15317=CARTESIAN_POINT('Ctrl Pts',(17.3130316956038,-10.7404136580229,1.1114114752902));
#15318=CARTESIAN_POINT('Ctrl Pts',(15.632337229038,-12.3448670237413,1.00027032776118));
#15319=CARTESIAN_POINT('Ctrl Pts',(13.3728188212649,-11.8029763021112,0.889129180232157));
#15320=CARTESIAN_POINT('Ctrl Pts',(12.6027721572564,-9.61060675361223,0.777988032703139));
#15321=CARTESIAN_POINT('Ctrl Pts',(14.0270251243106,-7.77487708517042,0.666846885174118));
#15322=CARTESIAN_POINT('Ctrl Pts',(16.3419550176155,-7.97554015919684,0.555705737645099));
#15323=CARTESIAN_POINT('Ctrl Pts',(17.4284073368472,-10.0300831221902,0.444564590116078));
#15324=CARTESIAN_POINT('Ctrl Pts',(16.2921947498604,-12.0555954005474,0.333423442587058));
#15325=CARTESIAN_POINT('Ctrl Pts',(13.9727681426279,-12.2024165492448,0.222282295058038));
#15326=CARTESIAN_POINT('Ctrl Pts',(12.5943476332648,-10.3273336439559,0.111141147529019));
#15327=CARTESIAN_POINT('Ctrl Pts',(13.1427287937432,-8.88671494767188,0.0370470491763388));
#15328=CARTESIAN_POINT('Ctrl Pts',(13.6609982804014,-8.44145197141313,-1.11022302462516E-15));
#15329=CARTESIAN_POINT('Ctrl Pts',(16.2690708798524,-8.92064134695149,8.));
#15330=CARTESIAN_POINT('Ctrl Pts',(16.3147846752501,-8.9632874663071,8.));
#15331=CARTESIAN_POINT('Ctrl Pts',(16.3577652736967,-9.00858426221366,8.));
#15332=CARTESIAN_POINT('Ctrl Pts',(16.3980010936161,-9.05619464640471,8.));
#15333=CARTESIAN_POINT('Ctrl Pts',(16.4235330189367,-9.08640615386467,8.));
#15334=CARTESIAN_POINT('Ctrl Pts',(16.4479592920189,-9.11755027257088,8.));
#15335=CARTESIAN_POINT('Ctrl Pts',(16.471271602956,-9.14954990813044,8.));
#15336=CARTESIAN_POINT('Ctrl Pts',(16.4873497379374,-9.17161955456194,8.));
#15337=CARTESIAN_POINT('Ctrl Pts',(16.502897912595,-9.19409628253225,8.));
#15338=CARTESIAN_POINT('Ctrl Pts',(16.5179120773105,-9.21695643030215,8.));
#15339=CARTESIAN_POINT('Ctrl Pts',(16.5257307264556,-9.22886088707372,8.));
#15340=CARTESIAN_POINT('Ctrl Pts',(16.5334041086722,-9.24086888444548,8.));
#15341=CARTESIAN_POINT('Ctrl Pts',(16.540924657522,-9.25296543092032,8.));
#15342=CARTESIAN_POINT('Ctrl Pts',(16.5757605428611,-9.30899776505104,8.));
#15343=CARTESIAN_POINT('Ctrl Pts',(16.607361406864,-9.36698896324546,8.));
#15344=CARTESIAN_POINT('Ctrl Pts',(16.6356943238752,-9.4265878438185,8.));
#15345=CARTESIAN_POINT('Ctrl Pts',(16.6561185797454,-9.46955069109315,8.));
#15346=CARTESIAN_POINT('Ctrl Pts',(16.6748440447478,-9.51335002846355,8.));
#15347=CARTESIAN_POINT('Ctrl Pts',(16.6918467496953,-9.55786627237312,8.));
#15348=CARTESIAN_POINT('Ctrl Pts',(16.6965928650873,-9.57029248520593,8.));
#15349=CARTESIAN_POINT('Ctrl Pts',(16.7012046820795,-9.58277460807998,8.));
#15350=CARTESIAN_POINT('Ctrl Pts',(16.7056815276087,-9.5953101474753,8.));
#15351=CARTESIAN_POINT('Ctrl Pts',(16.7100593754041,-9.60756848499157,8.));
#15352=CARTESIAN_POINT('Ctrl Pts',(16.7143051500548,-9.61986955747689,8.));
#15353=CARTESIAN_POINT('Ctrl Pts',(16.7184177206078,-9.63220775031721,8.));
#15354=CARTESIAN_POINT('Ctrl Pts',(16.7398746574473,-9.69658107135324,8.));
#15355=CARTESIAN_POINT('Ctrl Pts',(16.757717816168,-9.7619877167845,8.));
#15356=CARTESIAN_POINT('Ctrl Pts',(16.7719146523459,-9.8280714884005,8.));
#15357=CARTESIAN_POINT('Ctrl Pts',(16.7863151656955,-9.89510334137312,8.));
#15358=CARTESIAN_POINT('Ctrl Pts',(16.796964530901,-9.96283279931455,8.));
#15359=CARTESIAN_POINT('Ctrl Pts',(16.8037864817646,-10.0309197852966,8.));
#15360=CARTESIAN_POINT('Ctrl Pts',(16.8080119470385,-10.0730923544962,8.));
#15361=CARTESIAN_POINT('Ctrl Pts',(16.8107681716415,-10.1154026616984,8.));
#15362=CARTESIAN_POINT('Ctrl Pts',(16.8120276488193,-10.1577734446421,8.));
#15363=CARTESIAN_POINT('Ctrl Pts',(16.8130607162965,-10.1925274510017,8.));
#15364=CARTESIAN_POINT('Ctrl Pts',(16.813086670923,-10.2273222138279,8.));
#15365=CARTESIAN_POINT('Ctrl Pts',(16.8120863526574,-10.2621156498343,8.));
#15366=CARTESIAN_POINT('Ctrl Pts',(16.8116796422333,-10.2762620006526,8.));
#15367=CARTESIAN_POINT('Ctrl Pts',(16.8111029763007,-10.2904105498162,8.));
#15368=CARTESIAN_POINT('Ctrl Pts',(16.8103565468589,-10.304534652261,8.));
#15369=CARTESIAN_POINT('Ctrl Pts',(16.8066369705131,-10.3749172958421,8.));
#15370=CARTESIAN_POINT('Ctrl Pts',(16.7987037157801,-10.4448165407578,8.));
#15371=CARTESIAN_POINT('Ctrl Pts',(16.7864939545926,-10.5138749520222,8.));
#15372=CARTESIAN_POINT('Ctrl Pts',(16.7851389335045,-10.521538951517,8.));
#15373=CARTESIAN_POINT('Ctrl Pts',(16.7837311928168,-10.5291926144958,8.));
#15374=CARTESIAN_POINT('Ctrl Pts',(16.7822706091278,-10.5368354652215,8.));
#15375=CARTESIAN_POINT('Ctrl Pts',(16.7696155618455,-10.6030560029649,8.));
#15376=CARTESIAN_POINT('Ctrl Pts',(16.7529979131475,-10.6684646869657,8.));
#15377=CARTESIAN_POINT('Ctrl Pts',(16.7326887106986,-10.7328539224424,8.));
#15378=CARTESIAN_POINT('Ctrl Pts',(16.7108366552886,-10.8021346903597,8.));
#15379=CARTESIAN_POINT('Ctrl Pts',(16.6847110764563,-10.8702362184114,8.));
#15380=CARTESIAN_POINT('Ctrl Pts',(16.6545855938628,-10.9368941313461,8.));
#15381=CARTESIAN_POINT('Ctrl Pts',(16.6490331062011,-10.949179983962,8.));
#15382=CARTESIAN_POINT('Ctrl Pts',(16.6433445705813,-10.9614167555639,8.));
#15383=CARTESIAN_POINT('Ctrl Pts',(16.6375214788432,-10.9736027264117,8.));
#15384=CARTESIAN_POINT('Ctrl Pts',(16.6325870746563,-10.9839289428405,8.));
#15385=CARTESIAN_POINT('Ctrl Pts',(16.6275601738243,-10.9942100372499,8.));
#15386=CARTESIAN_POINT('Ctrl Pts',(16.6224425866455,-11.004444258572,8.));
#15387=CARTESIAN_POINT('Ctrl Pts',(16.5906566971579,-11.068010118141,8.));
#15388=CARTESIAN_POINT('Ctrl Pts',(16.5553718494201,-11.129778140702,8.));
#15389=CARTESIAN_POINT('Ctrl Pts',(16.5168961339094,-11.1895239538667,8.));
#15390=CARTESIAN_POINT('Ctrl Pts',(16.4776077060262,-11.2505317620566,8.));
#15391=CARTESIAN_POINT('Ctrl Pts',(16.4349918293265,-11.3094318958527,8.));
#15392=CARTESIAN_POINT('Ctrl Pts',(16.389322025044,-11.3659771816407,8.));
#15393=CARTESIAN_POINT('Ctrl Pts',(16.343374309462,-11.4228665585434,8.));
#15394=CARTESIAN_POINT('Ctrl Pts',(16.2943348495141,-11.4773732714099,8.));
#15395=CARTESIAN_POINT('Ctrl Pts',(16.2424345785477,-11.5292236977579,8.));
#15396=CARTESIAN_POINT('Ctrl Pts',(16.2296038331093,-11.5420421206477,8.));
#15397=CARTESIAN_POINT('Ctrl Pts',(16.216598038131,-11.5546980557672,8.));
#15398=CARTESIAN_POINT('Ctrl Pts',(16.2034202977729,-11.567187060214,8.));
#15399=CARTESIAN_POINT('Ctrl Pts',(16.1931258534052,-11.5769434644223,8.));
#15400=CARTESIAN_POINT('Ctrl Pts',(16.1827252138162,-11.5865989818742,8.));
#15401=CARTESIAN_POINT('Ctrl Pts',(16.1722359503905,-11.5961372133929,8.));
#15402=CARTESIAN_POINT('Ctrl Pts',(16.1164872924449,-11.6468312978828,8.));
#15403=CARTESIAN_POINT('Ctrl Pts',(16.0581412184438,-11.6943085897836,8.));
#15404=CARTESIAN_POINT('Ctrl Pts',(15.9974954853088,-11.7383155407977,8.));
#15405=CARTESIAN_POINT('Ctrl Pts',(15.9367829685185,-11.7823709526826,8.));
#15406=CARTESIAN_POINT('Ctrl Pts',(15.8737650860283,-11.8229493073405,8.));
#15407=CARTESIAN_POINT('Ctrl Pts',(15.808695859843,-11.859769768599,8.));
#15408=CARTESIAN_POINT('Ctrl Pts',(15.7451092258783,-11.8957512813619,8.));
#15409=CARTESIAN_POINT('Ctrl Pts',(15.679562930207,-11.9281449345628,8.));
#15410=CARTESIAN_POINT('Ctrl Pts',(15.6122617056636,-11.9566513041652,8.));
#15411=CARTESIAN_POINT('Ctrl Pts',(15.5977557447019,-11.9627955056625,8.));
#15412=CARTESIAN_POINT('Ctrl Pts',(15.5831681568552,-11.9687589532201,8.));
#15413=CARTESIAN_POINT('Ctrl Pts',(15.5685008393369,-11.9745383629168,8.));
#15414=CARTESIAN_POINT('Ctrl Pts',(15.5561465682195,-11.9794063555953,8.));
#15415=CARTESIAN_POINT('Ctrl Pts',(15.5437357303612,-11.9841437770524,8.));
#15416=CARTESIAN_POINT('Ctrl Pts',(15.5312701240486,-11.9887510481705,8.));
#15417=CARTESIAN_POINT('Ctrl Pts',(13.3326899541194,-10.0012996150481,6.87148036339021));
#15418=CARTESIAN_POINT('Ctrl Pts',(13.3319603302336,-10.0863816237079,6.87718308383007));
#15419=CARTESIAN_POINT('Ctrl Pts',(13.3379104914095,-10.1713612111695,6.88288580426994));
#15420=CARTESIAN_POINT('Ctrl Pts',(13.3508952182425,-10.25525186711,6.8885885247098));
#15421=CARTESIAN_POINT('Ctrl Pts',(13.4352489610918,-10.8002375960858,6.92563557388614));
#15422=CARTESIAN_POINT('Ctrl Pts',(13.8164823114028,-11.2992671739251,6.96268262306248));
#15423=CARTESIAN_POINT('Ctrl Pts',(14.3201120702849,-11.5239558890949,6.99972967223882));
#15424=CARTESIAN_POINT('Ctrl Pts',(14.8237418291669,-11.7486446042646,7.03677672141516));
#15425=CARTESIAN_POINT('Ctrl Pts',(15.44976799662,-11.6989924567648,7.0738237705915));
#15426=CARTESIAN_POINT('Ctrl Pts',(15.9116712180986,-11.397702424157,7.11087081976784));
#15427=CARTESIAN_POINT('Ctrl Pts',(16.3735744395772,-11.0964123915492,7.14791786894418));
#15428=CARTESIAN_POINT('Ctrl Pts',(16.6713547150814,-10.5434844738334,7.18496491812052));
#15429=CARTESIAN_POINT('Ctrl Pts',(16.6687230323053,-9.99202516121352,7.22201196729686));
#15430=CARTESIAN_POINT('Ctrl Pts',(16.6660913495291,-9.4405658485936,7.2590590164732));
#15431=CARTESIAN_POINT('Ctrl Pts',(16.3630477084726,-8.89057514106954,7.29610606564954));
#15432=CARTESIAN_POINT('Ctrl Pts',(15.8982908742206,-8.59369089292705,7.33315311482588));
#15433=CARTESIAN_POINT('Ctrl Pts',(15.4335340399686,-8.29680664478456,7.37020016400222));
#15434=CARTESIAN_POINT('Ctrl Pts',(14.8070640125211,-8.25302885602365,7.40724721317856));
#15435=CARTESIAN_POINT('Ctrl Pts',(14.3056004695722,-8.48255277528114,7.4442942623549));
#15436=CARTESIAN_POINT('Ctrl Pts',(13.8041369266233,-8.71207669453864,7.48134131153124));
#15437=CARTESIAN_POINT('Ctrl Pts',(13.4276798681731,-9.21490232181455,7.51838836070758));
#15438=CARTESIAN_POINT('Ctrl Pts',(13.3485326982206,-9.76058772075195,7.55543540988392));
#15439=CARTESIAN_POINT('Ctrl Pts',(13.3371065730611,-9.83936589651917,7.56078372771935));
#15440=CARTESIAN_POINT('Ctrl Pts',(13.3318768062629,-9.91903733051551,7.56613204555478));
#15441=CARTESIAN_POINT('Ctrl Pts',(13.3325429336747,-9.99879337075124,7.57148036339021));
#15442=CARTESIAN_POINT('Ctrl Pts',(14.4698297828114,-11.9851743256717,8.));
#15443=CARTESIAN_POINT('Ctrl Pts',(13.8096927451188,-11.8088749487748,7.96295295082366));
#15444=CARTESIAN_POINT('Ctrl Pts',(12.6905564701468,-10.7488614939858,7.88885885247098));
#15445=CARTESIAN_POINT('Ctrl Pts',(13.1189041392622,-8.4613875493231,7.77771770494197));
#15446=CARTESIAN_POINT('Ctrl Pts',(15.2723376840439,-7.58731246609672,7.66657655741293));
#15447=CARTESIAN_POINT('Ctrl Pts',(17.1748664515305,-8.91924865455582,7.55543540988393));
#15448=CARTESIAN_POINT('Ctrl Pts',(17.0874396573092,-11.2417232863365,7.44429426235489));
#15449=CARTESIAN_POINT('Ctrl Pts',(15.0888244971834,-12.4269237058338,7.33315311482589));
#15450=CARTESIAN_POINT('Ctrl Pts',(13.009124094798,-11.3909493747081,7.22201196729685));
#15451=CARTESIAN_POINT('Ctrl Pts',(12.7516786265559,-9.08158195460343,7.11087081976784));
#15452=CARTESIAN_POINT('Ctrl Pts',(14.5523165742456,-7.61298740370139,6.99972967223882));
#15453=CARTESIAN_POINT('Ctrl Pts',(16.7627158202625,-8.32932372056038,6.88858852470981));
#15454=CARTESIAN_POINT('Ctrl Pts',(17.3596103902574,-10.5749548405481,6.77744737718078));
#15455=CARTESIAN_POINT('Ctrl Pts',(15.7966027972857,-12.2942827529436,6.66630622965177));
#15456=CARTESIAN_POINT('Ctrl Pts',(13.5044206790732,-11.9135212765543,6.55516508212274));
#15457=CARTESIAN_POINT('Ctrl Pts',(12.5812305843409,-9.78119480556567,6.44402393459373));
#15458=CARTESIAN_POINT('Ctrl Pts',(13.8720874984692,-7.84915564699463,6.3328827870647));
#15459=CARTESIAN_POINT('Ctrl Pts',(16.1953903487128,-7.88591350252874,6.22174163953568));
#15460=CARTESIAN_POINT('Ctrl Pts',(17.4244804311674,-9.85782300540329,6.11060049200668));
#15461=CARTESIAN_POINT('Ctrl Pts',(16.4342968275999,-11.959875475957,5.99945934447763));
#15462=CARTESIAN_POINT('Ctrl Pts',(14.1312146931719,-12.2679355408755,5.88831819694863));
#15463=CARTESIAN_POINT('Ctrl Pts',(12.62338423969,-10.500017014522,5.7771770494196));
#15464=CARTESIAN_POINT('Ctrl Pts',(13.2910139128176,-8.27440271356362,5.66603590189059));
#15465=CARTESIAN_POINT('Ctrl Pts',(15.522981873134,-7.62833192925066,5.55489475436156));
#15466=CARTESIAN_POINT('Ctrl Pts',(17.2762329089047,-9.15319233958071,5.44375360683254));
#15467=CARTESIAN_POINT('Ctrl Pts',(16.9459103296842,-11.4531869986434,5.33261245930353));
#15468=CARTESIAN_POINT('Ctrl Pts',(14.8343783693084,-12.4229917343393,5.2214713117745));
#15469=CARTESIAN_POINT('Ctrl Pts',(12.8744499009111,-11.1748856301964,5.11033016424549));
#15470=CARTESIAN_POINT('Ctrl Pts',(12.86016595827,-8.85133567083148,4.99918901671646));
#15471=CARTESIAN_POINT('Ctrl Pts',(14.8046014971482,-7.57922762469993,4.88804786918745));
#15472=CARTESIAN_POINT('Ctrl Pts',(16.9278971004046,-8.52299890387884,4.77690672165843));
#15473=CARTESIAN_POINT('Ctrl Pts',(17.2864719188719,-10.8187585919275,4.6657655741294));
#15474=CARTESIAN_POINT('Ctrl Pts',(15.5521007403545,-12.3650590352537,4.55462442660039));
#15475=CARTESIAN_POINT('Ctrl Pts',(13.3123583718527,-11.7464779422144,4.44348327907137));
#15476=CARTESIAN_POINT('Ctrl Pts',(12.6174164274835,-9.52923998930584,4.33234213154235));
#15477=CARTESIAN_POINT('Ctrl Pts',(14.1033972880174,-7.74291713830186,4.22120098401333));
#15478=CARTESIAN_POINT('Ctrl Pts',(16.4100928231865,-8.02263870329727,4.1100598364843));
#15479=CARTESIAN_POINT('Ctrl Pts',(17.4260451371735,-10.1123586227095,3.99891868895528));
#15480=CARTESIAN_POINT('Ctrl Pts',(16.2212916482552,-12.0992299010838,3.88777754142627));
#15481=CARTESIAN_POINT('Ctrl Pts',(13.8986160692799,-12.1645491227624,3.77663639389725));
#15482=CARTESIAN_POINT('Ctrl Pts',(12.584103796379,-10.2485256546711,3.66549524636823));
#15483=CARTESIAN_POINT('Ctrl Pts',(13.4810073938554,-8.10501162795545,3.5543540988392));
#15484=CARTESIAN_POINT('Ctrl Pts',(15.7683367683932,-7.69609503710994,3.44321295131019));
#15485=CARTESIAN_POINT('Ctrl Pts',(17.3523610419581,-9.39608196253575,3.33207180378117));
#15486=CARTESIAN_POINT('Ctrl Pts',(16.7831270202232,-11.6488715830789,3.22093065625215));
#15487=CARTESIAN_POINT('Ctrl Pts',(14.5816890215374,-12.3923493459239,3.10978950872313));
#15488=CARTESIAN_POINT('Ctrl Pts',(12.7631563542956,-10.9459651010282,2.9986483611941));
#15489=CARTESIAN_POINT('Ctrl Pts',(12.9921419248582,-8.63368180206047,2.88750721366509));
#15490=CARTESIAN_POINT('Ctrl Pts',(15.0590413951949,-7.57207216315973,2.77636606613607));
#15491=CARTESIAN_POINT('Ctrl Pts',(17.0718967064505,-8.73289167567321,2.66522491860705));
#15492=CARTESIAN_POINT('Ctrl Pts',(17.1882196870663,-11.053572052764,2.55408377107803));
#15493=CARTESIAN_POINT('Ctrl Pts',(15.3015328785473,-12.4098542253325,2.44294262354901));
#15494=CARTESIAN_POINT('Ctrl Pts',(13.1388347955833,-11.5602511179916,2.33180147601999));
#15495=CARTESIAN_POINT('Ctrl Pts',(12.6797737556826,-9.2824558183502,2.22066032849097));
#15496=CARTESIAN_POINT('Ctrl Pts',(14.3445560924207,-7.66147210297657,2.10951918096195));
#15497=CARTESIAN_POINT('Ctrl Pts',(16.6093058597035,-8.18108435135386,1.99837803343293));
#15498=CARTESIAN_POINT('Ctrl Pts',(17.4009606855609,-10.3656601062701,1.88723688590391));
#15499=CARTESIAN_POINT('Ctrl Pts',(15.9948709901991,-12.2155249905566,1.77609573837489));
#15500=CARTESIAN_POINT('Ctrl Pts',(13.6781157885129,-12.0373860189781,1.66495459084587));
#15501=CARTESIAN_POINT('Ctrl Pts',(12.5713610061794,-9.99430418750461,1.55381344331685));
#15502=CARTESIAN_POINT('Ctrl Pts',(13.6876865848533,-7.95643655777695,1.44267229578783));
#15503=CARTESIAN_POINT('Ctrl Pts',(16.0052515070878,-7.78916517877589,1.33153114825881));
#15504=CARTESIAN_POINT('Ctrl Pts',(17.4026498601701,-9.64560639052843,1.22039000072979));
#15505=CARTESIAN_POINT('Ctrl Pts',(16.6007557452642,-11.8264420086883,1.10924885320077));
#15506=CARTESIAN_POINT('Ctrl Pts',(14.3335965506935,-12.3354315886432,0.998107705671752));
#15507=CARTESIAN_POINT('Ctrl Pts',(12.6764300571871,-10.7066463150279,0.88696655814273));
#15508=CARTESIAN_POINT('Ctrl Pts',(13.1461805475805,-8.43105034420652,0.775825410613713));
#15509=CARTESIAN_POINT('Ctrl Pts',(15.3128190350351,-7.59155964248331,0.664684263084691));
#15510=CARTESIAN_POINT('Ctrl Pts',(17.1931638558005,-8.95675538126231,0.553543115555674));
#15511=CARTESIAN_POINT('Ctrl Pts',(17.0658792003075,-11.2767112418142,0.442401968026652));
#15512=CARTESIAN_POINT('Ctrl Pts',(15.0477525273048,-12.4283740936836,0.331260820497633));
#15513=CARTESIAN_POINT('Ctrl Pts',(12.9855620345442,-11.3565055237641,0.220119672968612));
#15514=CARTESIAN_POINT('Ctrl Pts',(12.7679941505457,-9.04429144693358,0.108978525439592));
#15515=CARTESIAN_POINT('Ctrl Pts',(14.5921706189672,-7.6042694002394,-0.00216262208942743));
#15516=CARTESIAN_POINT('Ctrl Pts',(16.7924325358215,-8.36246876082203,-0.113303769618448));
#15517=CARTESIAN_POINT('Ctrl Pts',(17.160799328377,-9.85926548464068,-0.187397867971127));
#15518=CARTESIAN_POINT('Ctrl Pts',(16.9877912008532,-10.5202727210901,-0.224444917147467));
#15519=CARTESIAN_POINT('Ctrl Pts',(14.5032651029123,-11.8599788000028,8.07481497238249));
#15520=CARTESIAN_POINT('Ctrl Pts',(13.8847597760366,-11.6947977883195,8.03776792320615));
#15521=CARTESIAN_POINT('Ctrl Pts',(12.8362021159643,-10.7016343526812,7.96367382485347));
#15522=CARTESIAN_POINT('Ctrl Pts',(13.2375359299686,-8.55842053633704,7.85253267732444));
#15523=CARTESIAN_POINT('Ctrl Pts',(15.2551626384711,-7.73946922138811,7.74139152979544));
#15524=CARTESIAN_POINT('Ctrl Pts',(17.0377079435153,-8.98740651407504,7.6302503822664));
#15525=CARTESIAN_POINT('Ctrl Pts',(16.9557947423919,-11.1634136902684,7.51910923473739));
#15526=CARTESIAN_POINT('Ctrl Pts',(15.0832227575914,-12.2738691427251,7.40796808720837));
#15527=CARTESIAN_POINT('Ctrl Pts',(13.1346791920357,-11.303228797279,7.29682693967935));
#15528=CARTESIAN_POINT('Ctrl Pts',(12.8934695879748,-9.13950222311102,7.18568579215032));
#15529=CARTESIAN_POINT('Ctrl Pts',(14.5805498437857,-7.76352496249786,7.07454464462133));
#15530=CARTESIAN_POINT('Ctrl Pts',(16.6515496970314,-8.43468534665149,6.96340349709228));
#15531=CARTESIAN_POINT('Ctrl Pts',(17.2108009585808,-10.5386951667414,6.85226234956328));
#15532=CARTESIAN_POINT('Ctrl Pts',(15.7463648385,-12.1495932253925,6.74112120203425));
#15533=CARTESIAN_POINT('Ctrl Pts',(13.598739770773,-11.7928445687211,6.62998005450523));
#15534=CARTESIAN_POINT('Ctrl Pts',(12.7337708950579,-9.79499381101423,6.51883890697621));
#15535=CARTESIAN_POINT('Ctrl Pts',(13.9432195883374,-7.98479919523341,6.40769775944719));
#15536=CARTESIAN_POINT('Ctrl Pts',(16.1200027511848,-8.01923890722387,6.29655661191817));
#15537=CARTESIAN_POINT('Ctrl Pts',(17.2715799537993,-9.8667894338657,6.18541546438915));
#15538=CARTESIAN_POINT('Ctrl Pts',(16.3438425319874,-11.8362754287041,6.07427431686013));
#15539=CARTESIAN_POINT('Ctrl Pts',(14.1860048603503,-12.12490760698,5.9631331693311));
#15540=CARTESIAN_POINT('Ctrl Pts',(12.7732661193704,-10.4684833138455,5.8519920218021));
#15541=CARTESIAN_POINT('Ctrl Pts',(13.3987915567146,-8.38322794698246,5.74085087427306));
#15542=CARTESIAN_POINT('Ctrl Pts',(15.4899998877861,-7.77790178162586,5.62970972674406));
#15543=CARTESIAN_POINT('Ctrl Pts',(17.1326816993761,-9.20659648087737,5.51856857921503));
#15544=CARTESIAN_POINT('Ctrl Pts',(16.8231909979464,-11.3615413895713,5.40742743168601));
#15545=CARTESIAN_POINT('Ctrl Pts',(14.8448233397317,-12.2701851420167,5.29628628415699));
#15546=CARTESIAN_POINT('Ctrl Pts',(13.008498260569,-11.1007911679765,5.18514513662798));
#15547=CARTESIAN_POINT('Ctrl Pts',(12.9951151384173,-8.92377648000767,5.07400398909895));
#15548=CARTESIAN_POINT('Ctrl Pts',(14.8169243536164,-7.73189425257807,4.96286284156993));
#15549=CARTESIAN_POINT('Ctrl Pts',(16.8063137775701,-8.61614635508818,4.85172169404091));
#15550=CARTESIAN_POINT('Ctrl Pts',(17.1422749835657,-10.7671233722962,4.74058054651189));
#15551=CARTESIAN_POINT('Ctrl Pts',(15.5172823662112,-12.2159059833894,4.62943939898287));
#15552=CARTESIAN_POINT('Ctrl Pts',(13.4187899219914,-11.636335864908,4.51829825145386));
#15553=CARTESIAN_POINT('Ctrl Pts',(12.7676746687644,-9.55892858956661,4.40715710392483));
#15554=CARTESIAN_POINT('Ctrl Pts',(14.1599417669537,-7.88526064521431,4.29601595639582));
#15555=CARTESIAN_POINT('Ctrl Pts',(16.3211649592917,-8.14734149829962,4.18487480886679));
#15556=CARTESIAN_POINT('Ctrl Pts',(17.2730459812216,-10.1052726974829,4.07373366133778));
#15557=CARTESIAN_POINT('Ctrl Pts',(16.1442705786589,-11.9668414314328,3.96259251380876));
#15558=CARTESIAN_POINT('Ctrl Pts',(13.9680751280571,-12.0280412797201,3.85145136627974));
#15559=CARTESIAN_POINT('Ctrl Pts',(12.7364629072453,-10.23285232081,3.74031021875071));
#15560=CARTESIAN_POINT('Ctrl Pts',(13.5768030503649,-8.22451955343418,3.6291690712217));
#15561=CARTESIAN_POINT('Ctrl Pts',(15.7198814139359,-7.84139139178789,3.51802792369267));
#15562=CARTESIAN_POINT('Ctrl Pts',(17.2040087922828,-9.43416820775037,3.40688677616366));
#15563=CARTESIAN_POINT('Ctrl Pts',(16.6706736594555,-11.5448850757306,3.29574562863463));
#15564=CARTESIAN_POINT('Ctrl Pts',(14.6080699101901,-12.2414752236498,3.18460448110562));
#15565=CARTESIAN_POINT('Ctrl Pts',(12.9042234698843,-10.8863075704243,3.0734633335766));
#15566=CARTESIAN_POINT('Ctrl Pts',(13.1187680069787,-8.71984900803833,2.96232218604758));
#15567=CARTESIAN_POINT('Ctrl Pts',(15.0553179345335,-7.72519005204671,2.85118103851856));
#15568=CARTESIAN_POINT('Ctrl Pts',(16.9412320116973,-8.81280218564314,2.74003989098954));
#15569=CARTESIAN_POINT('Ctrl Pts',(17.0502190538429,-10.9871282622765,2.62889874346052));
#15570=CARTESIAN_POINT('Ctrl Pts',(15.2825166305796,-12.2578761533695,2.5177575959315));
#15571=CARTESIAN_POINT('Ctrl Pts',(13.2562096543604,-11.461853482899,2.40661644840248));
#15572=CARTESIAN_POINT('Ctrl Pts',(12.8260994161406,-9.32770792535695,2.29547530087346));
#15573=CARTESIAN_POINT('Ctrl Pts',(14.3858918297888,-7.80895196183496,2.18433415334444));
#15574=CARTESIAN_POINT('Ctrl Pts',(16.5078145748011,-8.29579473110992,2.07319300581542));
#15575=CARTESIAN_POINT('Ctrl Pts',(17.2495434869541,-10.3425996583141,1.9620518582864));
#15576=CARTESIAN_POINT('Ctrl Pts',(15.9321291972088,-12.0758023413976,1.85091071075738));
#15577=CARTESIAN_POINT('Ctrl Pts',(13.761480753791,-11.908897749541,1.73976956322836));
#15578=CARTESIAN_POINT('Ctrl Pts',(12.7245237443629,-9.9946633953738,1.62862841569934));
#15579=CARTESIAN_POINT('Ctrl Pts',(13.7704479654167,-8.08531440798811,1.51748726817032));
#15580=CARTESIAN_POINT('Ctrl Pts',(15.9418550641498,-7.92859204120862,1.4063461206413));
#15581=CARTESIAN_POINT('Ctrl Pts',(17.2511261333354,-9.6679563139874,1.29520497311228));
#15582=CARTESIAN_POINT('Ctrl Pts',(16.4998036755118,-11.7112569771147,1.18406382558326));
#15583=CARTESIAN_POINT('Ctrl Pts',(14.3756234543587,-12.1881469992633,1.07292267805424));
#15584=CARTESIAN_POINT('Ctrl Pts',(12.8229665888444,-10.6620814847619,0.961781530525221));
#15585=CARTESIAN_POINT('Ctrl Pts',(13.2630921446325,-8.5299965548063,0.850640382996201));
#15586=CARTESIAN_POINT('Ctrl Pts',(15.2930910227271,-7.74344854851155,0.73949923546718));
#15587=CARTESIAN_POINT('Ctrl Pts',(17.0548514173136,-9.02254786948623,0.628358087938162));
#15588=CARTESIAN_POINT('Ctrl Pts',(16.9355940011155,-11.1961951214013,0.517216940409141));
#15589=CARTESIAN_POINT('Ctrl Pts',(15.0447410019789,-12.2752280614948,0.406075792880122));
#15590=CARTESIAN_POINT('Ctrl Pts',(13.1126030791273,-11.2709571565884,0.294934645351101));
#15591=CARTESIAN_POINT('Ctrl Pts',(12.9087561692788,-9.10456345082775,0.18379349782208));
#15592=CARTESIAN_POINT('Ctrl Pts',(14.617890483002,-7.75535676214991,0.0726523502930618));
#15593=CARTESIAN_POINT('Ctrl Pts',(16.679392320337,-8.46574008648703,-0.0384887972359591));
#15594=CARTESIAN_POINT('Ctrl Pts',(17.0245279670749,-9.86814094278172,-0.112582895588638));
#15595=CARTESIAN_POINT('Ctrl Pts',(16.8624306412829,-10.4874615891075,-0.149629944764978));
#15596=CARTESIAN_POINT('Ctrl Pts',(14.5367004230132,-11.7347832743338,8.14962994476498));
#15597=CARTESIAN_POINT('Ctrl Pts',(13.9598268069544,-11.5807206278643,8.11258289558864));
#15598=CARTESIAN_POINT('Ctrl Pts',(12.9818477617818,-10.6544072113766,8.03848879723596));
#15599=CARTESIAN_POINT('Ctrl Pts',(13.356167720675,-8.65545352335096,7.92734764970694));
#15600=CARTESIAN_POINT('Ctrl Pts',(15.2379875928983,-7.89162597667949,7.81620650217792));
#15601=CARTESIAN_POINT('Ctrl Pts',(16.9005494355002,-9.05556437359427,7.7050653546489));
#15602=CARTESIAN_POINT('Ctrl Pts',(16.8241498274746,-11.0851040942002,7.59392420711988));
#15603=CARTESIAN_POINT('Ctrl Pts',(15.0776210179994,-12.1208145796164,7.48278305959086));
#15604=CARTESIAN_POINT('Ctrl Pts',(13.2602342892733,-11.2155082198498,7.37164191206184));
#15605=CARTESIAN_POINT('Ctrl Pts',(13.0352605493937,-9.19742249161861,7.26050076453282));
#15606=CARTESIAN_POINT('Ctrl Pts',(14.6087831133256,-7.91406252129431,7.1493596170038));
#15607=CARTESIAN_POINT('Ctrl Pts',(16.5403835738004,-8.5400469727426,7.03821846947478));
#15608=CARTESIAN_POINT('Ctrl Pts',(17.0619915269041,-10.5024354929347,6.92707732194576));
#15609=CARTESIAN_POINT('Ctrl Pts',(15.6961268797143,-12.0049036978414,6.81593617441673));
#15610=CARTESIAN_POINT('Ctrl Pts',(13.6930588624727,-11.672167860888,6.70479502688773));
#15611=CARTESIAN_POINT('Ctrl Pts',(12.886311205775,-9.80879281646281,6.59365387935869));
#15612=CARTESIAN_POINT('Ctrl Pts',(14.0143516782056,-8.12044274347216,6.48251273182969));
#15613=CARTESIAN_POINT('Ctrl Pts',(16.0446151536567,-8.152564311919,6.37137158430066));
#15614=CARTESIAN_POINT('Ctrl Pts',(17.1186794764312,-9.87575586232812,6.26023043677165));
#15615=CARTESIAN_POINT('Ctrl Pts',(16.2533882363748,-11.7126753814513,6.14908928924262));
#15616=CARTESIAN_POINT('Ctrl Pts',(14.2407950275287,-11.9818796730845,6.03794814171361));
#15617=CARTESIAN_POINT('Ctrl Pts',(12.9231479990509,-10.4369496131689,5.92680699418458));
#15618=CARTESIAN_POINT('Ctrl Pts',(13.5065692006116,-8.49205318040131,5.81566584665556));
#15619=CARTESIAN_POINT('Ctrl Pts',(15.4570179024382,-7.92747163400105,5.70452469912655));
#15620=CARTESIAN_POINT('Ctrl Pts',(16.9891304898475,-9.26000062217405,5.59338355159752));
#15621=CARTESIAN_POINT('Ctrl Pts',(16.7004716662086,-11.2698957804992,5.48224240406851));
#15622=CARTESIAN_POINT('Ctrl Pts',(14.8552683101549,-12.1173785496942,5.37110125653948));
#15623=CARTESIAN_POINT('Ctrl Pts',(13.1425466202268,-11.0266967057566,5.25996010901047));
#15624=CARTESIAN_POINT('Ctrl Pts',(13.1300643185645,-8.99621728918384,5.14881896148144));
#15625=CARTESIAN_POINT('Ctrl Pts',(14.8292472100845,-7.88456088045623,5.03767781395242));
#15626=CARTESIAN_POINT('Ctrl Pts',(16.6847304547357,-8.70929380629751,4.9265366664234));
#15627=CARTESIAN_POINT('Ctrl Pts',(16.9980780482594,-10.715488152665,4.81539551889438));
#15628=CARTESIAN_POINT('Ctrl Pts',(15.4824639920679,-12.066752931525,4.70425437136536));
#15629=CARTESIAN_POINT('Ctrl Pts',(13.5252214721301,-11.5261937876016,4.59311322383634));
#15630=CARTESIAN_POINT('Ctrl Pts',(12.9179329100453,-9.58861718982735,4.48197207630733));
#15631=CARTESIAN_POINT('Ctrl Pts',(14.21648624589,-8.02760415212678,4.3708309287783));
#15632=CARTESIAN_POINT('Ctrl Pts',(16.2322370953968,-8.27204429330195,4.25968978124928));
#15633=CARTESIAN_POINT('Ctrl Pts',(17.1200468252698,-10.0981867722562,4.14854863372027));
#15634=CARTESIAN_POINT('Ctrl Pts',(16.0672495090626,-11.8344529617818,4.03740748619125));
#15635=CARTESIAN_POINT('Ctrl Pts',(14.0375341868343,-11.8915334366777,3.92626633866222));
#15636=CARTESIAN_POINT('Ctrl Pts',(12.8888220181116,-10.2171789869489,3.81512519113321));
#15637=CARTESIAN_POINT('Ctrl Pts',(13.6725987068744,-8.34402747891293,3.70398404360418));
#15638=CARTESIAN_POINT('Ctrl Pts',(15.6714260594787,-7.98668774646583,3.59284289607517));
#15639=CARTESIAN_POINT('Ctrl Pts',(17.0556565426075,-9.47225445296499,3.48170174854615));
#15640=CARTESIAN_POINT('Ctrl Pts',(16.5582202986879,-11.4408985683823,3.37056060101712));
#15641=CARTESIAN_POINT('Ctrl Pts',(14.6344507988427,-12.0906011013757,3.25941945348811));
#15642=CARTESIAN_POINT('Ctrl Pts',(13.045290585473,-10.8266500398205,3.14827830595908));
#15643=CARTESIAN_POINT('Ctrl Pts',(13.2453940890993,-8.80601621401618,3.03713715843007));
#15644=CARTESIAN_POINT('Ctrl Pts',(15.0515944738721,-7.87830794093373,2.92599601090105));
#15645=CARTESIAN_POINT('Ctrl Pts',(16.810567316944,-8.89271269561304,2.81485486337202));
#15646=CARTESIAN_POINT('Ctrl Pts',(16.9122184206196,-10.9206844717891,2.70371371584301));
#15647=CARTESIAN_POINT('Ctrl Pts',(15.2635003826118,-12.1058980814064,2.59257256831398));
#15648=CARTESIAN_POINT('Ctrl Pts',(13.3735845131376,-11.3634558478065,2.48143142078497));
#15649=CARTESIAN_POINT('Ctrl Pts',(12.9724250765987,-9.3729600323637,2.37029027325594));
#15650=CARTESIAN_POINT('Ctrl Pts',(14.4272275671569,-7.95643182069336,2.25914912572693));
#15651=CARTESIAN_POINT('Ctrl Pts',(16.4063232898986,-8.41050511086595,2.14800797819791));
#15652=CARTESIAN_POINT('Ctrl Pts',(17.0981262883473,-10.3195392103582,2.03686683066889));
#15653=CARTESIAN_POINT('Ctrl Pts',(15.8693874042187,-11.9360796922385,1.92572568313987));
#15654=CARTESIAN_POINT('Ctrl Pts',(13.8448457190691,-11.7804094801039,1.81458453561085));
#15655=CARTESIAN_POINT('Ctrl Pts',(12.8776864825464,-9.99502260324298,1.70344338808183));
#15656=CARTESIAN_POINT('Ctrl Pts',(13.8532093459802,-8.21419225819928,1.59230224055281));
#15657=CARTESIAN_POINT('Ctrl Pts',(15.8784586212119,-8.06801890364133,1.48116109302379));
#15658=CARTESIAN_POINT('Ctrl Pts',(17.0996024065006,-9.69030623744639,1.37001994549477));
#15659=CARTESIAN_POINT('Ctrl Pts',(16.3988516057594,-11.5960719455411,1.25887879796575));
#15660=CARTESIAN_POINT('Ctrl Pts',(14.4176503580238,-12.0408624098834,1.14773765043673));
#15661=CARTESIAN_POINT('Ctrl Pts',(12.9695031205017,-10.6175166544959,1.03659650290771));
#15662=CARTESIAN_POINT('Ctrl Pts',(13.3800037416846,-8.62894276540608,0.92545535537869));
#15663=CARTESIAN_POINT('Ctrl Pts',(15.273363010419,-7.8953374545398,0.81431420784967));
#15664=CARTESIAN_POINT('Ctrl Pts',(16.9165389788268,-9.08834035771014,0.703173060320651));
#15665=CARTESIAN_POINT('Ctrl Pts',(16.8053088019234,-11.1156790009884,0.59203191279163));
#15666=CARTESIAN_POINT('Ctrl Pts',(15.0417294766531,-12.1220820293061,0.480890765262611));
#15667=CARTESIAN_POINT('Ctrl Pts',(13.2396441237103,-11.1854087894126,0.36974961773359));
#15668=CARTESIAN_POINT('Ctrl Pts',(13.0495181880118,-9.16483545472189,0.25860847020457));
#15669=CARTESIAN_POINT('Ctrl Pts',(14.6436103470368,-7.90644412406044,0.14746732267555));
#15670=CARTESIAN_POINT('Ctrl Pts',(16.5663521048524,-8.56901141215202,0.0363261751465301));
#15671=CARTESIAN_POINT('Ctrl Pts',(16.8882566057727,-9.87701640092277,-0.0377679232061492));
#15672=CARTESIAN_POINT('Ctrl Pts',(16.7370700817125,-10.4546504571249,-0.0748149723824891));
#15673=CARTESIAN_POINT('Ctrl Pts',(14.5701357431141,-11.6095877486648,8.22444491714747));
#15674=CARTESIAN_POINT('Ctrl Pts',(14.0348938378722,-11.4666434674091,8.18739786797113));
#15675=CARTESIAN_POINT('Ctrl Pts',(13.1274934075993,-10.6071800700719,8.11330376961845));
#15676=CARTESIAN_POINT('Ctrl Pts',(13.4747995113813,-8.75248651036489,8.00216262208942));
#15677=CARTESIAN_POINT('Ctrl Pts',(15.2208125473255,-8.04378273197088,7.89102147456042));
#15678=CARTESIAN_POINT('Ctrl Pts',(16.763390927485,-9.1237222331135,7.77988032703139));
#15679=CARTESIAN_POINT('Ctrl Pts',(16.6925049125573,-11.006794498132,7.66873917950237));
#15680=CARTESIAN_POINT('Ctrl Pts',(15.0720192784074,-11.9677600165076,7.55759803197335));
#15681=CARTESIAN_POINT('Ctrl Pts',(13.385789386511,-11.1277876424206,7.44645688444433));
#15682=CARTESIAN_POINT('Ctrl Pts',(13.1770515108126,-9.2553427601262,7.33531573691531));
#15683=CARTESIAN_POINT('Ctrl Pts',(14.6370163828657,-8.06460008009077,7.22417458938628));
#15684=CARTESIAN_POINT('Ctrl Pts',(16.4292174505694,-8.64540859883372,7.11303344185728));
#15685=CARTESIAN_POINT('Ctrl Pts',(16.9131820952275,-10.4661758191279,7.00189229432824));
#15686=CARTESIAN_POINT('Ctrl Pts',(15.6458889209286,-11.8602141702903,6.89075114679924));
#15687=CARTESIAN_POINT('Ctrl Pts',(13.7873779541725,-11.5514911530548,6.7796099992702));
#15688=CARTESIAN_POINT('Ctrl Pts',(13.038851516492,-9.82259182191137,6.6684688517412));
#15689=CARTESIAN_POINT('Ctrl Pts',(14.0854837680738,-8.25608629171094,6.55732770421216));
#15690=CARTESIAN_POINT('Ctrl Pts',(15.9692275561287,-8.28588971661412,6.44618655668316));
#15691=CARTESIAN_POINT('Ctrl Pts',(16.9657789990631,-9.88472229079055,6.33504540915413));
#15692=CARTESIAN_POINT('Ctrl Pts',(16.1629339407623,-11.5890753341985,6.22390426162511));
#15693=CARTESIAN_POINT('Ctrl Pts',(14.295585194707,-11.838851739189,6.11276311409609));
#15694=CARTESIAN_POINT('Ctrl Pts',(13.0730298787315,-10.4054159124924,6.00162196656708));
#15695=CARTESIAN_POINT('Ctrl Pts',(13.6143468445086,-8.60087841382016,5.89048081903805));
#15696=CARTESIAN_POINT('Ctrl Pts',(15.4240359170902,-8.07704148637625,5.77933967150903));
#15697=CARTESIAN_POINT('Ctrl Pts',(16.8455792803189,-9.31340476347071,5.66819852398002));
#15698=CARTESIAN_POINT('Ctrl Pts',(16.5777523344708,-11.1782501714271,5.55705737645098));
#15699=CARTESIAN_POINT('Ctrl Pts',(14.8657132805781,-11.9645719573716,5.44591622892198));
#15700=CARTESIAN_POINT('Ctrl Pts',(13.2765949798846,-10.9526022435367,5.33477508139295));
#15701=CARTESIAN_POINT('Ctrl Pts',(13.2650134987117,-9.06865809836003,5.22363393386394));
#15702=CARTESIAN_POINT('Ctrl Pts',(14.8415700665526,-8.03722750833437,5.11249278633491));
#15703=CARTESIAN_POINT('Ctrl Pts',(16.5631471319012,-8.80244125750684,5.00135163880589));
#15704=CARTESIAN_POINT('Ctrl Pts',(16.8538811129532,-10.6638529330338,4.89021049127687));
#15705=CARTESIAN_POINT('Ctrl Pts',(15.4476456179246,-11.9175998796606,4.77906934374785));
#15706=CARTESIAN_POINT('Ctrl Pts',(13.6316530222687,-11.4160517102953,4.66792819621883));
#15707=CARTESIAN_POINT('Ctrl Pts',(13.0681911513262,-9.61830579008811,4.55678704868982));
#15708=CARTESIAN_POINT('Ctrl Pts',(14.2730307248264,-8.16994765903925,4.44564590116079));
#15709=CARTESIAN_POINT('Ctrl Pts',(16.143309231502,-8.39674708830429,4.33450475363177));
#15710=CARTESIAN_POINT('Ctrl Pts',(16.9670476693179,-10.0911008470296,4.22336360610275));
#15711=CARTESIAN_POINT('Ctrl Pts',(15.9902284394662,-11.7020644921307,4.11222245857374));
#15712=CARTESIAN_POINT('Ctrl Pts',(14.1069932456115,-11.7550255936353,4.00108131104471));
#15713=CARTESIAN_POINT('Ctrl Pts',(13.0411811289779,-10.2015056530877,3.88994016351569));
#15714=CARTESIAN_POINT('Ctrl Pts',(13.7683943633839,-8.46353540439168,3.77879901598667));
#15715=CARTESIAN_POINT('Ctrl Pts',(15.6229707050215,-8.13198410114376,3.66765786845766));
#15716=CARTESIAN_POINT('Ctrl Pts',(16.9073042929321,-9.51034069817962,3.55651672092863));
#15717=CARTESIAN_POINT('Ctrl Pts',(16.4457669379203,-11.3369120610339,3.44537557339962));
#15718=CARTESIAN_POINT('Ctrl Pts',(14.6608316874954,-11.9397269791017,3.33423442587059));
#15719=CARTESIAN_POINT('Ctrl Pts',(13.1863577010617,-10.7669925092167,3.22309327834158));
#15720=CARTESIAN_POINT('Ctrl Pts',(13.3720201712198,-8.89218341999404,3.11195213081255));
#15721=CARTESIAN_POINT('Ctrl Pts',(15.0478710132107,-8.03142582982071,3.00081098328354));
#15722=CARTESIAN_POINT('Ctrl Pts',(16.6799026221908,-8.97262320558296,2.88966983575451));
#15723=CARTESIAN_POINT('Ctrl Pts',(16.7742177873962,-10.8542406813017,2.7785286882255));
#15724=CARTESIAN_POINT('Ctrl Pts',(15.2444841346441,-11.9539200094434,2.66738754069648));
#15725=CARTESIAN_POINT('Ctrl Pts',(13.4909593719147,-11.2650582127139,2.55624639316746));
#15726=CARTESIAN_POINT('Ctrl Pts',(13.1187507370567,-9.41821213937045,2.44510524563843));
#15727=CARTESIAN_POINT('Ctrl Pts',(14.4685633045251,-8.10391167955175,2.33396409810942));
#15728=CARTESIAN_POINT('Ctrl Pts',(16.3048320049962,-8.52521549062199,2.2228229505804));
#15729=CARTESIAN_POINT('Ctrl Pts',(16.9467090897406,-10.2964787624023,2.11168180305138));
#15730=CARTESIAN_POINT('Ctrl Pts',(15.8066456112284,-11.7963570430794,2.00054065552236));
#15731=CARTESIAN_POINT('Ctrl Pts',(13.9282106843473,-11.6519212106668,1.88939950799334));
#15732=CARTESIAN_POINT('Ctrl Pts',(13.0308492207299,-9.99538181111215,1.77825836046432));
#15733=CARTESIAN_POINT('Ctrl Pts',(13.9359707265436,-8.34307010841046,1.6671172129353));
#15734=CARTESIAN_POINT('Ctrl Pts',(15.8150621782739,-8.20744576607403,1.55597606540628));
#15735=CARTESIAN_POINT('Ctrl Pts',(16.9480786796658,-9.71265616090539,1.44483491787726));
#15736=CARTESIAN_POINT('Ctrl Pts',(16.2978995360069,-11.4808869139675,1.33369377034824));
#15737=CARTESIAN_POINT('Ctrl Pts',(14.459677261689,-11.8935778205035,1.22255262281922));
#15738=CARTESIAN_POINT('Ctrl Pts',(13.116039652159,-10.5729518242299,1.1114114752902));
#15739=CARTESIAN_POINT('Ctrl Pts',(13.4969153387366,-8.72788897600587,1.00027032776118));
#15740=CARTESIAN_POINT('Ctrl Pts',(15.2536349981109,-8.04722636056805,0.889129180232159));
#15741=CARTESIAN_POINT('Ctrl Pts',(16.77822654034,-9.15413284593406,0.77798803270314));
#15742=CARTESIAN_POINT('Ctrl Pts',(16.6750236027314,-11.0351628805755,0.66684688517412));
#15743=CARTESIAN_POINT('Ctrl Pts',(15.0387179513273,-11.9689359971173,0.5557057376451));
#15744=CARTESIAN_POINT('Ctrl Pts',(13.3666851682933,-11.0998604222368,0.44456459011608));
#15745=CARTESIAN_POINT('Ctrl Pts',(13.1902802067449,-9.22510745861606,0.333423442587058));
#15746=CARTESIAN_POINT('Ctrl Pts',(14.6693302110716,-8.05753148597096,0.22228229505804));
#15747=CARTESIAN_POINT('Ctrl Pts',(16.4533118893679,-8.67228273781702,0.111141147529019));
#15748=CARTESIAN_POINT('Ctrl Pts',(16.7519852444706,-9.88589185906381,0.0370470491763399));
#15749=CARTESIAN_POINT('Ctrl Pts',(16.6117095221421,-10.4218393251423,0.));
#15750=CARTESIAN_POINT('Ctrl Pts',(13.3361815844527,-9.99906045492932,7.3785196366098));
#15751=CARTESIAN_POINT('Ctrl Pts',(13.3350653698557,-9.78304622671375,7.36411833671163));
#15752=CARTESIAN_POINT('Ctrl Pts',(13.3741037210664,-9.56741861718908,7.34971703681347));
#15753=CARTESIAN_POINT('Ctrl Pts',(13.4551686354378,-9.36895979383603,7.33531573691531));
#15754=CARTESIAN_POINT('Ctrl Pts',(13.6637064681636,-8.85842853344772,7.29826868773897));
#15755=CARTESIAN_POINT('Ctrl Pts',(14.1503614255146,-8.46151430676925,7.26122163856262));
#15756=CARTESIAN_POINT('Ctrl Pts',(14.6923890821408,-8.3598586132205,7.22417458938629));
#15757=CARTESIAN_POINT('Ctrl Pts',(15.2344167387669,-8.25820291967176,7.18712754020995));
#15758=CARTESIAN_POINT('Ctrl Pts',(15.8318170946681,-8.45180575925274,7.15008049103361));
#15759=CARTESIAN_POINT('Ctrl Pts',(16.2111780467284,-8.8520683824256,7.11303344185727));
#15760=CARTESIAN_POINT('Ctrl Pts',(16.5905389987887,-9.25233100559846,7.07598639268093));
#15761=CARTESIAN_POINT('Ctrl Pts',(16.7518605470081,-9.8592534123632,7.03893934350459));
#15762=CARTESIAN_POINT('Ctrl Pts',(16.621305792068,-10.3950543409393,7.00189229432825));
#15763=CARTESIAN_POINT('Ctrl Pts',(16.4907510371279,-10.9308552695154,6.96484524515191));
#15764=CARTESIAN_POINT('Ctrl Pts',(16.0683199790282,-11.3955347199029,6.92779819597557));
#15765=CARTESIAN_POINT('Ctrl Pts',(15.5473526221857,-11.5764206088907,6.89075114679923));
#15766=CARTESIAN_POINT('Ctrl Pts',(15.0263852653432,-11.7573064978785,6.85370409762289));
#15767=CARTESIAN_POINT('Ctrl Pts',(14.4068816097579,-11.6543988254667,6.81665704844655));
#15768=CARTESIAN_POINT('Ctrl Pts',(13.9723753756851,-11.3147951007368,6.77960999927021));
#15769=CARTESIAN_POINT('Ctrl Pts',(13.5771626776233,-11.0059026297031,6.74591321171674));
#15770=CARTESIAN_POINT('Ctrl Pts',(13.3350007187014,-10.5011884793045,6.71221642416327));
#15771=CARTESIAN_POINT('Ctrl Pts',(13.331821388128,-9.99913246339926,6.6785196366098));
#15772=CARTESIAN_POINT('Ctrl Pts',(13.1998077676745,-10.0021672449552,7.99999999904539));
#15773=CARTESIAN_POINT('Ctrl Pts',(13.2074798175735,-9.93506922612593,7.99999999936359));
#15774=CARTESIAN_POINT('Ctrl Pts',(13.2188240784654,-9.86823467174956,8.));
#15775=CARTESIAN_POINT('Ctrl Pts',(13.2338166554418,-9.80202407246294,8.));
#15776=CARTESIAN_POINT('Ctrl Pts',(13.2487940185892,-9.73588066087505,8.));
#15777=CARTESIAN_POINT('Ctrl Pts',(13.2673389547068,-9.67068097467151,8.));
#15778=CARTESIAN_POINT('Ctrl Pts',(13.2893701892982,-9.6067646838403,8.));
#15779=CARTESIAN_POINT('Ctrl Pts',(13.3109714057993,-9.54409594730352,8.));
#15780=CARTESIAN_POINT('Ctrl Pts',(13.3359247078376,-9.48266014999381,8.));
#15781=CARTESIAN_POINT('Ctrl Pts',(13.3641933030361,-9.42280701535511,8.));
#15782=CARTESIAN_POINT('Ctrl Pts',(13.3758894405641,-9.39804276763416,8.));
#15783=CARTESIAN_POINT('Ctrl Pts',(13.3881535513658,-9.37354987995325,8.));
#15784=CARTESIAN_POINT('Ctrl Pts',(13.4009847510562,-9.34935515259193,8.));
#15785=CARTESIAN_POINT('Ctrl Pts',(13.4067964172714,-9.33839657638825,8.));
#15786=CARTESIAN_POINT('Ctrl Pts',(13.4127244333369,-9.32749918518064,8.));
#15787=CARTESIAN_POINT('Ctrl Pts',(13.4187687789279,-9.31666556315984,8.));
#15788=CARTESIAN_POINT('Ctrl Pts',(13.425159640313,-9.30521086130789,8.));
#15789=CARTESIAN_POINT('Ctrl Pts',(13.431676443445,-9.2938348748043,8.));
#15790=CARTESIAN_POINT('Ctrl Pts',(13.4383166419856,-9.28254377672475,8.));
#15791=CARTESIAN_POINT('Ctrl Pts',(13.4709216418811,-9.22710172187461,8.));
#15792=CARTESIAN_POINT('Ctrl Pts',(13.5065145504896,-9.17367537459915,8.));
#15793=CARTESIAN_POINT('Ctrl Pts',(13.5450538037118,-9.12258927669459,8.));
#15794=CARTESIAN_POINT('Ctrl Pts',(13.5823769497808,-9.07311520195852,8.));
#15795=CARTESIAN_POINT('Ctrl Pts',(13.6224639480267,-9.02583549550675,8.));
#15796=CARTESIAN_POINT('Ctrl Pts',(13.6653053703033,-8.9810847385994,8.));
#15797=CARTESIAN_POINT('Ctrl Pts',(13.6782878320201,-8.96752368115845,8.));
#15798=CARTESIAN_POINT('Ctrl Pts',(13.6915234071565,-8.9541951706708,8.));
#15799=CARTESIAN_POINT('Ctrl Pts',(13.7050122636503,-8.94110937848357,8.));
#15800=CARTESIAN_POINT('Ctrl Pts',(13.7127736320724,-8.93357992968962,8.));
#15801=CARTESIAN_POINT('Ctrl Pts',(13.7206188601492,-8.92613084760238,8.));
#15802=CARTESIAN_POINT('Ctrl Pts',(13.7285464165792,-8.9187628208919,8.));
#15803=CARTESIAN_POINT('Ctrl Pts',(14.4698297828114,-11.9851743256717,8.));
#15804=CARTESIAN_POINT('Ctrl Pts',(14.3998214683822,-11.9592528423604,8.));
#15805=CARTESIAN_POINT('Ctrl Pts',(14.3314995298914,-11.9292588102101,8.));
#15806=CARTESIAN_POINT('Ctrl Pts',(14.2650832927778,-11.8954790830356,8.));
#15807=CARTESIAN_POINT('Ctrl Pts',(14.200410195712,-11.8625859281483,8.));
#15808=CARTESIAN_POINT('Ctrl Pts',(14.1375436561858,-11.8261022624894,8.));
#15809=CARTESIAN_POINT('Ctrl Pts',(14.0767171136307,-11.7862591514963,8.));
#15810=CARTESIAN_POINT('Ctrl Pts',(14.0631404357672,-11.7773660423319,8.));
#15811=CARTESIAN_POINT('Ctrl Pts',(14.0496637435695,-11.7683042245779,8.));
#15812=CARTESIAN_POINT('Ctrl Pts',(14.0362955933952,-11.7590800518159,8.));
#15813=CARTESIAN_POINT('Ctrl Pts',(13.9749538754163,-11.7167535820521,8.));
#15814=CARTESIAN_POINT('Ctrl Pts',(13.9160153064361,-11.6710962446947,8.));
#15815=CARTESIAN_POINT('Ctrl Pts',(13.8597184805936,-11.6223773773913,8.));
#15816=CARTESIAN_POINT('Ctrl Pts',(13.8201933952585,-11.5881726534344,8.));
#15817=CARTESIAN_POINT('Ctrl Pts',(13.7819712022528,-11.5524579711967,8.));
#15818=CARTESIAN_POINT('Ctrl Pts',(13.7451473327347,-11.5153181422045,8.));
#15819=CARTESIAN_POINT('Ctrl Pts',(13.7311386073503,-11.5011892178959,8.));
#15820=CARTESIAN_POINT('Ctrl Pts',(13.717332371766,-11.4868539850208,8.));
#15821=CARTESIAN_POINT('Ctrl Pts',(13.7037343400326,-11.4723169303692,8.));
#15822=CARTESIAN_POINT('Ctrl Pts',(13.6908095393624,-11.4584995972883,8.));
#15823=CARTESIAN_POINT('Ctrl Pts',(13.6780690151191,-11.4444953919844,8.));
#15824=CARTESIAN_POINT('Ctrl Pts',(13.6655396735727,-11.4303333656545,8.));
#15825=CARTESIAN_POINT('Ctrl Pts',(13.6174405812511,-11.3759665332569,8.));
#15826=CARTESIAN_POINT('Ctrl Pts',(13.5723959249184,-11.3192214581869,8.));
#15827=CARTESIAN_POINT('Ctrl Pts',(13.5306282578393,-11.2603460850308,8.));
#15828=CARTESIAN_POINT('Ctrl Pts',(13.4897585016075,-11.2027363999032,8.));
#15829=CARTESIAN_POINT('Ctrl Pts',(13.4520259976655,-11.1430861593352,8.));
#15830=CARTESIAN_POINT('Ctrl Pts',(13.4176843817239,-11.0816085238734,8.));
#15831=CARTESIAN_POINT('Ctrl Pts',(13.3840955339157,-11.0214784780236,8.));
#15832=CARTESIAN_POINT('Ctrl Pts',(13.3537502688523,-10.9595995550916,8.));
#15833=CARTESIAN_POINT('Ctrl Pts',(13.3269341460252,-10.8961642041122,8.));
#15834=CARTESIAN_POINT('Ctrl Pts',(13.3182225174315,-10.8755562578776,8.));
#15835=CARTESIAN_POINT('Ctrl Pts',(13.3098837493054,-10.8547840384658,8.));
#15836=CARTESIAN_POINT('Ctrl Pts',(13.3019288365863,-10.8338541688359,8.));
#15837=CARTESIAN_POINT('Ctrl Pts',(13.2974344402897,-10.8220291329271,8.));
#15838=CARTESIAN_POINT('Ctrl Pts',(13.2930622312048,-10.8101524909552,8.));
#15839=CARTESIAN_POINT('Ctrl Pts',(13.2888200152093,-10.7982424246399,8.));
#15840=CARTESIAN_POINT('Ctrl Pts',(13.265903681499,-10.7339045751566,8.));
#15841=CARTESIAN_POINT('Ctrl Pts',(13.2467331549497,-10.6684810537996,8.));
#15842=CARTESIAN_POINT('Ctrl Pts',(13.2315367307289,-10.6021713571593,8.));
#15843=CARTESIAN_POINT('Ctrl Pts',(13.2293393441876,-10.5925830465909,8.));
#15844=CARTESIAN_POINT('Ctrl Pts',(13.2272251395615,-10.5829761934059,8.));
#15845=CARTESIAN_POINT('Ctrl Pts',(13.2251948980547,-10.5733513897451,8.));
#15846=CARTESIAN_POINT('Ctrl Pts',(13.2108418424753,-10.5053075922838,8.));
#15847=CARTESIAN_POINT('Ctrl Pts',(13.2006809368273,-10.4363661073907,8.));
#15848=CARTESIAN_POINT('Ctrl Pts',(13.1946148801756,-10.3668853682355,8.));
#15849=CARTESIAN_POINT('Ctrl Pts',(13.1893452075922,-10.3065264287755,8.));
#15850=CARTESIAN_POINT('Ctrl Pts',(13.1871667948597,-10.245760095398,8.));
#15851=CARTESIAN_POINT('Ctrl Pts',(13.188045983141,-10.1848309054691,8.));
#15852=CARTESIAN_POINT('Ctrl Pts',(13.1882953481151,-10.1675495037619,8.));
#15853=CARTESIAN_POINT('Ctrl Pts',(13.1887908474924,-10.1502550857216,8.));
#15854=CARTESIAN_POINT('Ctrl Pts',(13.1895320856308,-10.1329534599018,8.));
#15855=CARTESIAN_POINT('Ctrl Pts',(13.1900857549631,-10.1200299753721,8.));
#15856=CARTESIAN_POINT('Ctrl Pts',(13.1907767641003,-10.1071003962073,8.));
#15857=CARTESIAN_POINT('Ctrl Pts',(13.1916034374083,-10.0941871331301,8.));
#15858=CARTESIAN_POINT('Ctrl Pts',(13.1935720387064,-10.0634360901101,8.));
#15859=CARTESIAN_POINT('Ctrl Pts',(13.1963106067788,-10.0327526423872,8.));
#15860=CARTESIAN_POINT('Ctrl Pts',(13.1998077693062,-10.0021672451286,8.));
#15861=CARTESIAN_POINT('Origin',(0.,0.,8.));
#15862=CARTESIAN_POINT('',(-12.,10.,8.));
#15863=CARTESIAN_POINT('',(-6.,10.,8.));
#15864=CARTESIAN_POINT('',(-16.,6.,8.));
#15865=CARTESIAN_POINT('',(-13.5,8.5,8.));
#15866=CARTESIAN_POINT('',(-16.,-5.,8.));
#15867=CARTESIAN_POINT('',(2.,4.,8.));
#15868=CARTESIAN_POINT('',(-2.,4.,8.));
#15869=CARTESIAN_POINT('',(1.,4.,8.));
#15870=CARTESIAN_POINT('',(-2.,6.,8.));
#15871=CARTESIAN_POINT('',(-2.,2.,8.));
#15872=CARTESIAN_POINT('',(2.,6.,8.));
#15873=CARTESIAN_POINT('',(-1.,6.,8.));
#15874=CARTESIAN_POINT('',(2.,3.,8.));
#15875=CARTESIAN_POINT('',(10.,-6.,8.));
#15876=CARTESIAN_POINT('',(6.,-6.,8.));
#15877=CARTESIAN_POINT('',(5.,-6.,8.));
#15878=CARTESIAN_POINT('',(6.,-4.,8.));
#15879=CARTESIAN_POINT('',(6.,-3.,8.));
#15880=CARTESIAN_POINT('',(10.,-4.,8.));
#15881=CARTESIAN_POINT('',(3.,-4.,8.));
#15882=CARTESIAN_POINT('',(10.,-2.,8.));
#15883=CARTESIAN_POINT('',(-6.,-6.,8.));
#15884=CARTESIAN_POINT('',(-10.,-6.,8.));
#15885=CARTESIAN_POINT('',(-3.,-6.,8.));
#15886=CARTESIAN_POINT('',(-10.,-4.,8.));
#15887=CARTESIAN_POINT('',(-10.,-3.,8.));
#15888=CARTESIAN_POINT('',(-6.,-4.,8.));
#15889=CARTESIAN_POINT('',(-5.,-4.,8.));
#15890=CARTESIAN_POINT('',(-6.,-2.,8.));
#15891=CARTESIAN_POINT('Origin',(15.,-10.,8.));
#15892=CARTESIAN_POINT('Origin',(15.,-10.,4.));
#15893=CARTESIAN_POINT('Origin',(-15.,-10.,8.));
#15894=CARTESIAN_POINT('',(-16.,-5.,8.));
#15895=CARTESIAN_POINT('Origin',(-15.,-10.,4.));
#15896=CARTESIAN_POINT('Origin',(-15.,10.,4.));
#15897=CARTESIAN_POINT('Origin',(-15.,10.,8.));
#15898=CARTESIAN_POINT('Origin',(15.,10.,4.));
#15899=CARTESIAN_POINT('Origin',(15.,10.,8.));
#15900=CARTESIAN_POINT('Origin',(-6.,-6.,8.));
#15901=CARTESIAN_POINT('',(-6.,-6.,8.));
#15902=CARTESIAN_POINT('',(-10.,-6.,8.));
#15903=CARTESIAN_POINT('Origin',(-6.,-4.,8.));
#15904=CARTESIAN_POINT('',(-6.,-4.,8.));
#15905=CARTESIAN_POINT('Origin',(-10.,-4.,8.));
#15906=CARTESIAN_POINT('',(-10.,-4.,8.));
#15907=CARTESIAN_POINT('Origin',(-10.,-6.,8.));
#15908=CARTESIAN_POINT('Origin',(10.,-6.,8.));
#15909=CARTESIAN_POINT('',(10.,-6.,8.));
#15910=CARTESIAN_POINT('',(6.,-6.,8.));
#15911=CARTESIAN_POINT('Origin',(10.,-4.,8.));
#15912=CARTESIAN_POINT('',(10.,-4.,8.));
#15913=CARTESIAN_POINT('Origin',(6.,-4.,8.));
#15914=CARTESIAN_POINT('',(6.,-4.,8.));
#15915=CARTESIAN_POINT('Origin',(6.,-6.,8.));
#15916=CARTESIAN_POINT('Origin',(2.,4.,8.));
#15917=CARTESIAN_POINT('',(2.,4.,8.));
#15918=CARTESIAN_POINT('',(-2.,4.,8.));
#15919=CARTESIAN_POINT('Origin',(2.,6.,8.));
#15920=CARTESIAN_POINT('',(2.,6.,8.));
#15921=CARTESIAN_POINT('Origin',(-2.,6.,8.));
#15922=CARTESIAN_POINT('',(-2.,6.,8.));
#15923=CARTESIAN_POINT('Origin',(-2.,4.,8.));
#15924=CARTESIAN_POINT('Origin',(0.,0.,24.));
#15925=CARTESIAN_POINT('',(-34.,-20.,24.));
#15926=CARTESIAN_POINT('',(-34.,20.,24.));
#15927=CARTESIAN_POINT('',(-34.,-20.,24.));
#15928=CARTESIAN_POINT('',(-20.,10.,24.));
#15929=CARTESIAN_POINT('',(-16.,14.,24.));
#15930=CARTESIAN_POINT('',(-15.5,14.5,24.));
#15931=CARTESIAN_POINT('',(-20.,-14.,24.));
#15932=CARTESIAN_POINT('',(-20.,5.,24.));
#15933=CARTESIAN_POINT('',(20.,-14.,24.));
#15934=CARTESIAN_POINT('',(-10.,-14.,24.));
#15935=CARTESIAN_POINT('',(20.,10.,24.));
#15936=CARTESIAN_POINT('',(20.,-7.,24.));
#15937=CARTESIAN_POINT('',(16.,14.,24.));
#15938=CARTESIAN_POINT('',(17.5,12.5,24.));
#15939=CARTESIAN_POINT('',(8.,14.,24.));
#15940=CARTESIAN_POINT('Origin',(-34.,-20.,24.));
#15941=CARTESIAN_POINT('',(-34.,-20.,24.));
#15942=CARTESIAN_POINT('Origin',(-34.,20.,24.));
#15943=CARTESIAN_POINT('Origin',(-12.,10.,0.));
#15944=CARTESIAN_POINT('',(-12.,10.,0.));
#15945=CARTESIAN_POINT('Origin',(-16.,6.,0.));
#15946=CARTESIAN_POINT('',(-16.,6.,0.));
#15947=CARTESIAN_POINT('Origin',(20.,-14.,0.));
#15948=CARTESIAN_POINT('',(20.,-14.,0.));
#15949=CARTESIAN_POINT('',(20.,10.,0.));
#15950=CARTESIAN_POINT('Origin',(-20.,-14.,0.));
#15951=CARTESIAN_POINT('',(-20.,-14.,0.));
#15952=CARTESIAN_POINT('Origin',(-20.,10.,0.));
#15953=CARTESIAN_POINT('',(-20.,10.,0.));
#15954=CARTESIAN_POINT('Origin',(-16.,-10.,0.));
#15955=CARTESIAN_POINT('Origin',(-16.,14.,0.));
#15956=CARTESIAN_POINT('',(-16.,14.,0.));
#15957=CARTESIAN_POINT('Origin',(16.,14.,0.));
#15958=CARTESIAN_POINT('',(16.,14.,0.));
#15959=CARTESIAN_POINT('Origin',(20.,10.,0.));
#15960=CARTESIAN_POINT('',(0.,0.,0.));
#15961=CARTESIAN_POINT('Origin',(39.,24.,2.));
#15962=CARTESIAN_POINT('',(40.,24.,2.));
#15963=CARTESIAN_POINT('',(39.,24.,3.));
#15964=CARTESIAN_POINT('Origin',(39.,24.,2.));
#15965=CARTESIAN_POINT('',(39.,25.,2.));
#15966=CARTESIAN_POINT('Origin',(39.,24.,2.));
#15967=CARTESIAN_POINT('Origin',(39.,24.,2.));
#15968=CARTESIAN_POINT('Origin',(-39.,24.,2.));
#15969=CARTESIAN_POINT('',(-39.,25.,2.));
#15970=CARTESIAN_POINT('',(-39.,24.,3.));
#15971=CARTESIAN_POINT('Origin',(-39.,24.,2.));
#15972=CARTESIAN_POINT('',(-40.,24.,2.));
#15973=CARTESIAN_POINT('Origin',(-39.,24.,2.));
#15974=CARTESIAN_POINT('Origin',(-39.,24.,2.));
#15975=CARTESIAN_POINT('Origin',(39.,24.,1.));
#15976=CARTESIAN_POINT('',(40.,24.,1.));
#15977=CARTESIAN_POINT('',(39.,25.,1.));
#15978=CARTESIAN_POINT('Origin',(39.,24.,1.));
#15979=CARTESIAN_POINT('',(39.,24.,0.));
#15980=CARTESIAN_POINT('Origin',(39.,24.,1.));
#15981=CARTESIAN_POINT('Origin',(39.,24.,1.));
#15982=CARTESIAN_POINT('Origin',(39.,-24.,2.));
#15983=CARTESIAN_POINT('',(39.,-25.,2.));
#15984=CARTESIAN_POINT('',(39.,-24.,3.));
#15985=CARTESIAN_POINT('Origin',(39.,-24.,2.));
#15986=CARTESIAN_POINT('',(40.,-24.,2.));
#15987=CARTESIAN_POINT('Origin',(39.,-24.,2.));
#15988=CARTESIAN_POINT('Origin',(39.,-24.,2.));
#15989=CARTESIAN_POINT('Origin',(-39.,24.,1.));
#15990=CARTESIAN_POINT('',(-39.,24.,0.));
#15991=CARTESIAN_POINT('',(-39.,25.,1.));
#15992=CARTESIAN_POINT('Origin',(-39.,24.,1.));
#15993=CARTESIAN_POINT('',(-40.,24.,1.));
#15994=CARTESIAN_POINT('Origin',(-39.,24.,1.));
#15995=CARTESIAN_POINT('Origin',(-39.,24.,1.));
#15996=CARTESIAN_POINT('Origin',(-39.,-24.,2.));
#15997=CARTESIAN_POINT('',(-40.,-24.,2.));
#15998=CARTESIAN_POINT('',(-39.,-24.,3.));
#15999=CARTESIAN_POINT('Origin',(-39.,-24.,2.));
#16000=CARTESIAN_POINT('',(-39.,-25.,2.));
#16001=CARTESIAN_POINT('Origin',(-39.,-24.,2.));
#16002=CARTESIAN_POINT('Origin',(-39.,-24.,2.));
#16003=CARTESIAN_POINT('Origin',(39.,-24.,1.));
#16004=CARTESIAN_POINT('',(39.,-25.,1.));
#16005=CARTESIAN_POINT('',(40.,-24.,1.));
#16006=CARTESIAN_POINT('Origin',(39.,-24.,1.));
#16007=CARTESIAN_POINT('',(39.,-24.,0.));
#16008=CARTESIAN_POINT('Origin',(39.,-24.,1.));
#16009=CARTESIAN_POINT('Origin',(39.,-24.,1.));
#16010=CARTESIAN_POINT('Origin',(-39.,-24.,1.));
#16011=CARTESIAN_POINT('',(-40.,-24.,1.));
#16012=CARTESIAN_POINT('',(-39.,-25.,1.));
#16013=CARTESIAN_POINT('Origin',(-39.,-24.,1.));
#16014=CARTESIAN_POINT('',(-39.,-24.,0.));
#16015=CARTESIAN_POINT('Origin',(-39.,-24.,1.));
#16016=CARTESIAN_POINT('Origin',(-39.,-24.,1.));
#16017=CARTESIAN_POINT('Origin',(-39.,12.5,1.));
#16018=CARTESIAN_POINT('',(-40.,12.5,1.));
#16019=CARTESIAN_POINT('',(-39.,12.5,0.));
#16020=CARTESIAN_POINT('Origin',(-20.,-24.,1.));
#16021=CARTESIAN_POINT('',(-20.,-25.,1.));
#16022=CARTESIAN_POINT('',(-20.,-24.,0.));
#16023=CARTESIAN_POINT('Origin',(-39.,-24.,0.));
#16024=CARTESIAN_POINT('',(-40.,-24.,0.));
#16025=CARTESIAN_POINT('',(-39.,-25.,0.));
#16026=CARTESIAN_POINT('Origin',(39.,-12.5,1.));
#16027=CARTESIAN_POINT('',(40.,-12.5,1.));
#16028=CARTESIAN_POINT('',(39.,-12.5,0.));
#16029=CARTESIAN_POINT('Origin',(39.,-24.,0.));
#16030=CARTESIAN_POINT('',(39.,-25.,0.));
#16031=CARTESIAN_POINT('',(40.,-24.,0.));
#16032=CARTESIAN_POINT('Origin',(-20.,-24.,2.));
#16033=CARTESIAN_POINT('',(-20.,-24.,3.));
#16034=CARTESIAN_POINT('',(-20.,-25.,2.));
#16035=CARTESIAN_POINT('Origin',(-39.,12.5,2.));
#16036=CARTESIAN_POINT('',(-39.,12.5,3.));
#16037=CARTESIAN_POINT('',(-40.,12.5,2.));
#16038=CARTESIAN_POINT('Origin',(-39.,24.,0.));
#16039=CARTESIAN_POINT('',(-39.,25.,0.));
#16040=CARTESIAN_POINT('',(-40.,24.,0.));
#16041=CARTESIAN_POINT('Origin',(20.,24.,1.));
#16042=CARTESIAN_POINT('',(20.,25.,1.));
#16043=CARTESIAN_POINT('',(20.,24.,0.));
#16044=CARTESIAN_POINT('Origin',(39.,-12.5,2.));
#16045=CARTESIAN_POINT('',(39.,-12.5,3.));
#16046=CARTESIAN_POINT('',(40.,-12.5,2.));
#16047=CARTESIAN_POINT('Origin',(39.,24.,0.));
#16048=CARTESIAN_POINT('',(40.,24.,0.));
#16049=CARTESIAN_POINT('',(39.,25.,0.));
#16050=CARTESIAN_POINT('Origin',(20.,24.,2.));
#16051=CARTESIAN_POINT('',(20.,24.,3.));
#16052=CARTESIAN_POINT('',(20.,25.,2.));
#16053=CARTESIAN_POINT('Origin',(-40.,25.,0.));
#16054=CARTESIAN_POINT('Origin',(0.,0.,0.));
#16055=CARTESIAN_POINT('',(-21.,-15.,0.));
#16056=CARTESIAN_POINT('',(21.,-15.,0.));
#16057=CARTESIAN_POINT('',(10.5,-15.,0.));
#16058=CARTESIAN_POINT('',(21.,15.,0.));
#16059=CARTESIAN_POINT('',(21.,7.5,0.));
#16060=CARTESIAN_POINT('',(-21.,15.,0.));
#16061=CARTESIAN_POINT('',(-10.5,15.,0.));
#16062=CARTESIAN_POINT('',(-21.,-7.5,0.));
#16063=CARTESIAN_POINT('',(24.5,4.28626379701574E-16,0.));
#16064=CARTESIAN_POINT('Origin',(28.,0.,0.));
#16065=CARTESIAN_POINT('',(-31.5,4.28626379701574E-16,0.));
#16066=CARTESIAN_POINT('Origin',(-28.,0.,0.));
#16067=CARTESIAN_POINT('Origin',(-40.,-25.,0.));
#16068=CARTESIAN_POINT('Origin',(40.,-25.,0.));
#16069=CARTESIAN_POINT('Origin',(0.,0.,3.));
#16070=CARTESIAN_POINT('',(21.,-15.,3.));
#16071=CARTESIAN_POINT('',(-21.,-15.,3.));
#16072=CARTESIAN_POINT('',(10.5,-15.,3.));
#16073=CARTESIAN_POINT('',(-21.,15.,3.));
#16074=CARTESIAN_POINT('',(-21.,-7.5,3.));
#16075=CARTESIAN_POINT('',(21.,15.,3.));
#16076=CARTESIAN_POINT('',(-10.5,15.,3.));
#16077=CARTESIAN_POINT('',(21.,7.5,3.));
#16078=CARTESIAN_POINT('',(24.5,4.28626379701574E-16,3.));
#16079=CARTESIAN_POINT('Origin',(28.,0.,3.));
#16080=CARTESIAN_POINT('',(-31.5,4.28626379701574E-16,3.));
#16081=CARTESIAN_POINT('Origin',(-28.,0.,3.));
#16082=CARTESIAN_POINT('Origin',(40.,25.,0.));
#16083=CARTESIAN_POINT('Origin',(-28.,0.,1.5));
#16084=CARTESIAN_POINT('',(-31.5,4.28626379701574E-16,1.5));
#16085=CARTESIAN_POINT('Origin',(28.,0.,1.5));
#16086=CARTESIAN_POINT('',(24.5,4.28626379701574E-16,1.5));
#16087=CARTESIAN_POINT('Origin',(21.,-15.,3.));
#16088=CARTESIAN_POINT('',(21.,-15.,3.));
#16089=CARTESIAN_POINT('',(-21.,-15.,3.));
#16090=CARTESIAN_POINT('Origin',(21.,15.,3.));
#16091=CARTESIAN_POINT('',(21.,15.,3.));
#16092=CARTESIAN_POINT('Origin',(-21.,15.,3.));
#16093=CARTESIAN_POINT('',(-21.,15.,3.));
#16094=CARTESIAN_POINT('Origin',(-21.,-15.,3.));
#16095=CARTESIAN_POINT('',(0.,0.,0.));
#16096=CARTESIAN_POINT('Origin',(-28.,0.,0.5));
#16097=CARTESIAN_POINT('',(-31.5,4.28626379701574E-16,1.));
#16098=CARTESIAN_POINT('Origin',(-28.,0.,1.));
#16099=CARTESIAN_POINT('',(-31.5,4.28626379701574E-16,0.));
#16100=CARTESIAN_POINT('',(-31.5,4.28626379701574E-16,0.5));
#16101=CARTESIAN_POINT('Origin',(-28.,0.,0.));
#16102=CARTESIAN_POINT('Origin',(28.,0.,0.5));
#16103=CARTESIAN_POINT('',(24.5,4.28626379701574E-16,1.));
#16104=CARTESIAN_POINT('Origin',(28.,0.,1.));
#16105=CARTESIAN_POINT('',(24.5,4.28626379701574E-16,0.));
#16106=CARTESIAN_POINT('',(24.5,4.28626379701574E-16,0.5));
#16107=CARTESIAN_POINT('Origin',(28.,0.,0.));
#16108=CARTESIAN_POINT('Origin',(21.,-15.,0.));
#16109=CARTESIAN_POINT('',(21.,-15.,0.));
#16110=CARTESIAN_POINT('',(-21.,-15.,0.));
#16111=CARTESIAN_POINT('',(-21.,-15.,0.));
#16112=CARTESIAN_POINT('',(-21.,-15.,1.));
#16113=CARTESIAN_POINT('',(-21.,-15.,0.));
#16114=CARTESIAN_POINT('',(21.,-15.,1.));
#16115=CARTESIAN_POINT('',(-21.,-15.,1.));
#16116=CARTESIAN_POINT('',(21.,-15.,0.));
#16117=CARTESIAN_POINT('Origin',(21.,15.,0.));
#16118=CARTESIAN_POINT('',(21.,15.,0.));
#16119=CARTESIAN_POINT('',(21.,-15.,0.));
#16120=CARTESIAN_POINT('',(21.,15.,1.));
#16121=CARTESIAN_POINT('',(21.,-15.,1.));
#16122=CARTESIAN_POINT('',(21.,15.,0.));
#16123=CARTESIAN_POINT('Origin',(-21.,15.,0.));
#16124=CARTESIAN_POINT('',(-21.,15.,0.));
#16125=CARTESIAN_POINT('',(21.,15.,0.));
#16126=CARTESIAN_POINT('',(-21.,15.,1.));
#16127=CARTESIAN_POINT('',(21.,15.,1.));
#16128=CARTESIAN_POINT('',(-21.,15.,0.));
#16129=CARTESIAN_POINT('Origin',(-21.,-15.,0.));
#16130=CARTESIAN_POINT('',(-21.,15.,0.));
#16131=CARTESIAN_POINT('',(-21.,15.,1.));
#16132=CARTESIAN_POINT('Origin',(34.,20.,0.));
#16133=CARTESIAN_POINT('',(34.,20.,0.));
#16134=CARTESIAN_POINT('',(-34.,20.,0.));
#16135=CARTESIAN_POINT('',(34.,20.,0.));
#16136=CARTESIAN_POINT('',(-34.,20.,1.));
#16137=CARTESIAN_POINT('',(-34.,20.,0.));
#16138=CARTESIAN_POINT('',(34.,20.,1.));
#16139=CARTESIAN_POINT('',(34.,20.,1.));
#16140=CARTESIAN_POINT('',(34.,20.,0.));
#16141=CARTESIAN_POINT('Origin',(34.,-20.,0.));
#16142=CARTESIAN_POINT('',(34.,-20.,0.));
#16143=CARTESIAN_POINT('',(34.,-20.,0.));
#16144=CARTESIAN_POINT('',(34.,-20.,1.));
#16145=CARTESIAN_POINT('',(34.,-20.,1.));
#16146=CARTESIAN_POINT('',(34.,-20.,0.));
#16147=CARTESIAN_POINT('Origin',(-34.,-20.,0.));
#16148=CARTESIAN_POINT('',(-34.,-20.,0.));
#16149=CARTESIAN_POINT('',(-34.,-20.,0.));
#16150=CARTESIAN_POINT('',(-34.,-20.,1.));
#16151=CARTESIAN_POINT('',(-34.,-20.,1.));
#16152=CARTESIAN_POINT('',(-34.,-20.,0.));
#16153=CARTESIAN_POINT('Origin',(-34.,20.,0.));
#16154=CARTESIAN_POINT('',(-34.,20.,0.));
#16155=CARTESIAN_POINT('',(-34.,20.,1.));
#16156=CARTESIAN_POINT('Origin',(0.,0.,1.));
#16157=CARTESIAN_POINT('Origin',(0.,0.,0.));
#16158=CARTESIAN_POINT('',(0.,0.,0.));
#16159=CARTESIAN_POINT('Origin',(15.,-10.,1.5));
#16160=CARTESIAN_POINT('',(12.5,-10.,3.));
#16161=CARTESIAN_POINT('Origin',(15.,-10.,3.));
#16162=CARTESIAN_POINT('',(12.5,-10.,0.));
#16163=CARTESIAN_POINT('',(12.5,-10.,1.5));
#16164=CARTESIAN_POINT('Origin',(15.,-10.,0.));
#16165=CARTESIAN_POINT('Origin',(-15.,-10.,1.5));
#16166=CARTESIAN_POINT('',(-17.5,-10.,3.));
#16167=CARTESIAN_POINT('Origin',(-15.,-10.,3.));
#16168=CARTESIAN_POINT('',(-17.5,-10.,0.));
#16169=CARTESIAN_POINT('',(-17.5,-10.,1.5));
#16170=CARTESIAN_POINT('Origin',(-15.,-10.,0.));
#16171=CARTESIAN_POINT('Origin',(-15.,10.,1.5));
#16172=CARTESIAN_POINT('',(-17.5,10.,3.));
#16173=CARTESIAN_POINT('Origin',(-15.,10.,3.));
#16174=CARTESIAN_POINT('',(-17.5,10.,0.));
#16175=CARTESIAN_POINT('',(-17.5,10.,1.5));
#16176=CARTESIAN_POINT('Origin',(-15.,10.,0.));
#16177=CARTESIAN_POINT('Origin',(15.,10.,1.5));
#16178=CARTESIAN_POINT('',(12.5,10.,3.));
#16179=CARTESIAN_POINT('Origin',(15.,10.,3.));
#16180=CARTESIAN_POINT('',(12.5,10.,0.));
#16181=CARTESIAN_POINT('',(12.5,10.,1.5));
#16182=CARTESIAN_POINT('Origin',(15.,10.,0.));
#16183=CARTESIAN_POINT('Origin',(-6.,-6.,3.));
#16184=CARTESIAN_POINT('',(-6.,-6.,3.));
#16185=CARTESIAN_POINT('',(-10.,-6.,3.));
#16186=CARTESIAN_POINT('',(-3.,-6.,3.));
#16187=CARTESIAN_POINT('',(-6.,-6.,0.));
#16188=CARTESIAN_POINT('',(-6.,-6.,3.));
#16189=CARTESIAN_POINT('',(-10.,-6.,0.));
#16190=CARTESIAN_POINT('',(-3.,-6.,0.));
#16191=CARTESIAN_POINT('',(-10.,-6.,3.));
#16192=CARTESIAN_POINT('Origin',(-6.,-4.,3.));
#16193=CARTESIAN_POINT('',(-6.,-4.,3.));
#16194=CARTESIAN_POINT('',(-6.,-2.,3.));
#16195=CARTESIAN_POINT('',(-6.,-4.,0.));
#16196=CARTESIAN_POINT('',(-6.,-4.,3.));
#16197=CARTESIAN_POINT('',(-6.,-2.,0.));
#16198=CARTESIAN_POINT('Origin',(-10.,-4.,3.));
#16199=CARTESIAN_POINT('',(-10.,-4.,3.));
#16200=CARTESIAN_POINT('',(-5.,-4.,3.));
#16201=CARTESIAN_POINT('',(-10.,-4.,0.));
#16202=CARTESIAN_POINT('',(-10.,-4.,3.));
#16203=CARTESIAN_POINT('',(-5.,-4.,0.));
#16204=CARTESIAN_POINT('Origin',(-10.,-6.,3.));
#16205=CARTESIAN_POINT('',(-10.,-3.,3.));
#16206=CARTESIAN_POINT('',(-10.,-3.,0.));
#16207=CARTESIAN_POINT('Origin',(10.,-6.,3.));
#16208=CARTESIAN_POINT('',(10.,-6.,3.));
#16209=CARTESIAN_POINT('',(6.,-6.,3.));
#16210=CARTESIAN_POINT('',(5.,-6.,3.));
#16211=CARTESIAN_POINT('',(10.,-6.,0.));
#16212=CARTESIAN_POINT('',(10.,-6.,3.));
#16213=CARTESIAN_POINT('',(6.,-6.,0.));
#16214=CARTESIAN_POINT('',(5.,-6.,0.));
#16215=CARTESIAN_POINT('',(6.,-6.,3.));
#16216=CARTESIAN_POINT('Origin',(10.,-4.,3.));
#16217=CARTESIAN_POINT('',(10.,-4.,3.));
#16218=CARTESIAN_POINT('',(10.,-2.,3.));
#16219=CARTESIAN_POINT('',(10.,-4.,0.));
#16220=CARTESIAN_POINT('',(10.,-4.,3.));
#16221=CARTESIAN_POINT('',(10.,-2.,0.));
#16222=CARTESIAN_POINT('Origin',(6.,-4.,3.));
#16223=CARTESIAN_POINT('',(6.,-4.,3.));
#16224=CARTESIAN_POINT('',(3.,-4.,3.));
#16225=CARTESIAN_POINT('',(6.,-4.,0.));
#16226=CARTESIAN_POINT('',(6.,-4.,3.));
#16227=CARTESIAN_POINT('',(3.,-4.,0.));
#16228=CARTESIAN_POINT('Origin',(6.,-6.,3.));
#16229=CARTESIAN_POINT('',(6.,-3.,3.));
#16230=CARTESIAN_POINT('',(6.,-3.,0.));
#16231=CARTESIAN_POINT('Origin',(2.,4.,3.));
#16232=CARTESIAN_POINT('',(2.,4.,3.));
#16233=CARTESIAN_POINT('',(-2.,4.,3.));
#16234=CARTESIAN_POINT('',(1.,4.,3.));
#16235=CARTESIAN_POINT('',(2.,4.,0.));
#16236=CARTESIAN_POINT('',(2.,4.,3.));
#16237=CARTESIAN_POINT('',(-2.,4.,0.));
#16238=CARTESIAN_POINT('',(1.,4.,0.));
#16239=CARTESIAN_POINT('',(-2.,4.,3.));
#16240=CARTESIAN_POINT('Origin',(2.,6.,3.));
#16241=CARTESIAN_POINT('',(2.,6.,3.));
#16242=CARTESIAN_POINT('',(2.,3.,3.));
#16243=CARTESIAN_POINT('',(2.,6.,0.));
#16244=CARTESIAN_POINT('',(2.,6.,3.));
#16245=CARTESIAN_POINT('',(2.,3.,0.));
#16246=CARTESIAN_POINT('Origin',(-2.,6.,3.));
#16247=CARTESIAN_POINT('',(-2.,6.,3.));
#16248=CARTESIAN_POINT('',(-1.,6.,3.));
#16249=CARTESIAN_POINT('',(-2.,6.,0.));
#16250=CARTESIAN_POINT('',(-2.,6.,3.));
#16251=CARTESIAN_POINT('',(-1.,6.,0.));
#16252=CARTESIAN_POINT('Origin',(-2.,4.,3.));
#16253=CARTESIAN_POINT('',(-2.,2.,3.));
#16254=CARTESIAN_POINT('',(-2.,2.,0.));
#16255=CARTESIAN_POINT('Origin',(20.,14.,0.));
#16256=CARTESIAN_POINT('',(20.,14.,0.));
#16257=CARTESIAN_POINT('',(-20.,14.,0.));
#16258=CARTESIAN_POINT('',(20.,14.,0.));
#16259=CARTESIAN_POINT('',(-20.,14.,3.));
#16260=CARTESIAN_POINT('',(-20.,14.,0.));
#16261=CARTESIAN_POINT('',(20.,14.,3.));
#16262=CARTESIAN_POINT('',(20.,14.,3.));
#16263=CARTESIAN_POINT('',(20.,14.,0.));
#16264=CARTESIAN_POINT('Origin',(20.,-14.,0.));
#16265=CARTESIAN_POINT('',(20.,-14.,0.));
#16266=CARTESIAN_POINT('',(20.,-14.,0.));
#16267=CARTESIAN_POINT('',(20.,-14.,3.));
#16268=CARTESIAN_POINT('',(20.,-14.,3.));
#16269=CARTESIAN_POINT('',(20.,-14.,0.));
#16270=CARTESIAN_POINT('Origin',(-20.,-14.,0.));
#16271=CARTESIAN_POINT('',(-20.,-14.,0.));
#16272=CARTESIAN_POINT('',(-20.,-14.,0.));
#16273=CARTESIAN_POINT('',(-20.,-14.,3.));
#16274=CARTESIAN_POINT('',(-20.,-14.,3.));
#16275=CARTESIAN_POINT('',(-20.,-14.,0.));
#16276=CARTESIAN_POINT('Origin',(-20.,14.,0.));
#16277=CARTESIAN_POINT('',(-20.,14.,0.));
#16278=CARTESIAN_POINT('',(-20.,14.,3.));
#16279=CARTESIAN_POINT('Origin',(0.,0.,3.));
#16280=CARTESIAN_POINT('Origin',(0.,0.,0.));
#16281=CARTESIAN_POINT('',(0.,0.,0.));
#16282=CARTESIAN_POINT('Origin',(0.,0.,2.));
#16283=CARTESIAN_POINT('',(1.22464679914735E-16,1.,1.));
#16284=CARTESIAN_POINT('Origin',(0.,1.,2.));
#16285=CARTESIAN_POINT('',(1.22464679914735E-16,-1.,1.));
#16286=CARTESIAN_POINT('',(1.22464679914735E-16,0.,1.));
#16287=CARTESIAN_POINT('Origin',(0.,-1.,2.));
#16288=CARTESIAN_POINT('Origin',(2.,1.,0.));
#16289=CARTESIAN_POINT('',(2.,1.,0.));
#16290=CARTESIAN_POINT('',(-2.,1.,0.));
#16291=CARTESIAN_POINT('',(2.,1.,0.));
#16292=CARTESIAN_POINT('',(-2.,1.,28.));
#16293=CARTESIAN_POINT('',(-2.,1.,0.));
#16294=CARTESIAN_POINT('',(2.,1.,28.));
#16295=CARTESIAN_POINT('',(2.,1.,28.));
#16296=CARTESIAN_POINT('',(2.,1.,0.));
#16297=CARTESIAN_POINT('Origin',(2.,-1.,0.));
#16298=CARTESIAN_POINT('',(2.,-1.,0.));
#16299=CARTESIAN_POINT('',(2.,-1.,0.));
#16300=CARTESIAN_POINT('',(2.,-1.,28.));
#16301=CARTESIAN_POINT('',(2.,-1.,28.));
#16302=CARTESIAN_POINT('',(2.,-1.,0.));
#16303=CARTESIAN_POINT('Origin',(-2.,-1.,0.));
#16304=CARTESIAN_POINT('',(-2.,-1.,0.));
#16305=CARTESIAN_POINT('',(-2.,-1.,0.));
#16306=CARTESIAN_POINT('',(-2.,-1.,28.));
#16307=CARTESIAN_POINT('',(-2.,-1.,28.));
#16308=CARTESIAN_POINT('',(-2.,-1.,0.));
#16309=CARTESIAN_POINT('Origin',(-2.,1.,0.));
#16310=CARTESIAN_POINT('',(-2.,1.,0.));
#16311=CARTESIAN_POINT('',(-2.,1.,28.));
#16312=CARTESIAN_POINT('Origin',(0.,0.,28.));
#16313=CARTESIAN_POINT('Origin',(0.,0.,0.));
#16314=CARTESIAN_POINT('',(0.,0.,0.));
#16315=CARTESIAN_POINT('Origin',(0.,0.,2.));
#16316=CARTESIAN_POINT('',(1.22464679914735E-16,1.,1.));
#16317=CARTESIAN_POINT('Origin',(0.,1.,2.));
#16318=CARTESIAN_POINT('',(1.22464679914735E-16,-1.,1.));
#16319=CARTESIAN_POINT('',(1.22464679914735E-16,0.,1.));
#16320=CARTESIAN_POINT('Origin',(0.,-1.,2.));
#16321=CARTESIAN_POINT('Origin',(2.,1.,0.));
#16322=CARTESIAN_POINT('',(2.,1.,0.));
#16323=CARTESIAN_POINT('',(-2.,1.,0.));
#16324=CARTESIAN_POINT('',(2.,1.,0.));
#16325=CARTESIAN_POINT('',(-2.,1.,24.));
#16326=CARTESIAN_POINT('',(-2.,1.,0.));
#16327=CARTESIAN_POINT('',(2.,1.,24.));
#16328=CARTESIAN_POINT('',(2.,1.,24.));
#16329=CARTESIAN_POINT('',(2.,1.,0.));
#16330=CARTESIAN_POINT('Origin',(2.,-1.,0.));
#16331=CARTESIAN_POINT('',(2.,-1.,0.));
#16332=CARTESIAN_POINT('',(2.,-1.,0.));
#16333=CARTESIAN_POINT('',(2.,-1.,24.));
#16334=CARTESIAN_POINT('',(2.,-1.,24.));
#16335=CARTESIAN_POINT('',(2.,-1.,0.));
#16336=CARTESIAN_POINT('Origin',(-2.,-1.,0.));
#16337=CARTESIAN_POINT('',(-2.,-1.,0.));
#16338=CARTESIAN_POINT('',(-2.,-1.,0.));
#16339=CARTESIAN_POINT('',(-2.,-1.,24.));
#16340=CARTESIAN_POINT('',(-2.,-1.,24.));
#16341=CARTESIAN_POINT('',(-2.,-1.,0.));
#16342=CARTESIAN_POINT('Origin',(-2.,1.,0.));
#16343=CARTESIAN_POINT('',(-2.,1.,0.));
#16344=CARTESIAN_POINT('',(-2.,1.,24.));
#16345=CARTESIAN_POINT('Origin',(0.,0.,24.));
#16346=CARTESIAN_POINT('Origin',(0.,0.,0.));
#16347=CARTESIAN_POINT('',(0.,0.,0.));
#16348=CARTESIAN_POINT('Origin',(0.,0.,0.));
#16349=CARTESIAN_POINT('',(-1.95633598837559,0.00127248296362327,0.22586969212423));
#16350=CARTESIAN_POINT('',(-1.95588590413641,0.00206796222160181,0.124130307875766));
#16351=CARTESIAN_POINT('',(-1.954,-2.39295984553393E-16,0.));
#16352=CARTESIAN_POINT('',(0.861525859670522,1.75382131162755,0.));
#16353=CARTESIAN_POINT('Ctrl Pts',(-1.95633598837559,0.00127248296362327,
0.22586969212423));
#16354=CARTESIAN_POINT('Ctrl Pts',(-1.95680065536751,0.06824838727295,0.222037687723474));
#16355=CARTESIAN_POINT('Ctrl Pts',(-1.95366001618977,0.135177367276064,
0.218205683322718));
#16356=CARTESIAN_POINT('Ctrl Pts',(-1.9467704464542,0.201714622162032,0.214373678921962));
#16357=CARTESIAN_POINT('Ctrl Pts',(-1.88018097341933,0.844814396182631,
0.177336365489126));
#16358=CARTESIAN_POINT('Ctrl Pts',(-1.46337681650964,1.45132029737704,0.140299052056291));
#16359=CARTESIAN_POINT('Ctrl Pts',(-0.886898775458456,1.74452597744752,
0.103261738623455));
#16360=CARTESIAN_POINT('Ctrl Pts',(-0.351149650411554,2.01701629862282,
0.0688411590823035));
#16361=CARTESIAN_POINT('Ctrl Pts',(0.32250805655704,2.01891265608728,0.0344205795411517));
#16362=CARTESIAN_POINT('Ctrl Pts',(0.863568564283469,1.75641400930303,6.50521303491303E-18));
#16363=CARTESIAN_POINT('',(-0.861525859670545,1.75382131162753,0.));
#16364=CARTESIAN_POINT('Origin',(0.,0.,0.));
#16365=CARTESIAN_POINT('Ctrl Pts',(-0.861525859670546,1.75382131162753,
1.07552855510562E-15));
#16366=CARTESIAN_POINT('Ctrl Pts',(-1.44517400349648,1.46711709294739,0.0370752371124262));
#16367=CARTESIAN_POINT('Ctrl Pts',(-1.86938639577653,0.868642989156275,
0.0741504742248514));
#16368=CARTESIAN_POINT('Ctrl Pts',(-1.94388330047271,0.2267475072264,0.111225711337276));
#16369=CARTESIAN_POINT('Ctrl Pts',(-1.95252655828524,0.15227369973538,0.115527243516773));
#16370=CARTESIAN_POINT('Ctrl Pts',(-1.95646228341413,0.0772153955205521,
0.119828775696269));
#16371=CARTESIAN_POINT('Ctrl Pts',(-1.95588590413641,0.00206796222160181,
0.124130307875766));
#16372=CARTESIAN_POINT('Origin',(0.,0.,0.));
#16373=CARTESIAN_POINT('',(-1.95128265771456,0.000979968443958618,0.92586969212423));
#16374=CARTESIAN_POINT('',(-1.95120671878141,0.0009421225145049,0.824130307875766));
#16375=CARTESIAN_POINT('',(-1.954,-2.39295984553393E-16,0.));
#16376=CARTESIAN_POINT('Ctrl Pts',(-1.95128265771456,0.000979968443958618,
0.92586969212423));
#16377=CARTESIAN_POINT('Ctrl Pts',(-1.95247392016078,0.26388492489574,0.910928234987155));
#16378=CARTESIAN_POINT('Ctrl Pts',(-1.90305890226364,0.526360198569273,
0.895986777850081));
#16379=CARTESIAN_POINT('Ctrl Pts',(-1.80091082202569,0.76639335768976,0.881045320713007));
#16380=CARTESIAN_POINT('Ctrl Pts',(-1.54770322455863,1.36139445209842,0.844008007280172));
#16381=CARTESIAN_POINT('Ctrl Pts',(-0.970472477077253,1.8184979102298,0.806970693847336));
#16382=CARTESIAN_POINT('Ctrl Pts',(-0.333275819998743,1.92861264524847,
0.7699333804145));
#16383=CARTESIAN_POINT('Ctrl Pts',(0.303920837079767,2.03872738026714,0.732896066981664));
#16384=CARTESIAN_POINT('Ctrl Pts',(1.00108340375541,1.8018533921731,0.695858753548828));
#16385=CARTESIAN_POINT('Ctrl Pts',(1.43928269883041,1.32632160988724,0.658821440115992));
#16386=CARTESIAN_POINT('Ctrl Pts',(1.87748199390539,0.850789827601394,0.621784126683156));
#16387=CARTESIAN_POINT('Ctrl Pts',(2.05671801737973,0.13660025112374,0.584746813250321));
#16388=CARTESIAN_POINT('Ctrl Pts',(1.89500736899678,-0.489477875405323,
0.547709499817485));
#16389=CARTESIAN_POINT('Ctrl Pts',(1.73329672061383,-1.11555600193439,0.510672186384649));
#16390=CARTESIAN_POINT('Ctrl Pts',(1.23063940037359,-1.65352267851487,0.473634872951813));
#16391=CARTESIAN_POINT('Ctrl Pts',(0.616962143929708,-1.85738653188124,
0.436597559518977));
#16392=CARTESIAN_POINT('Ctrl Pts',(0.00328488748583246,-2.06125038524761,
0.399560246086142));
#16393=CARTESIAN_POINT('Ctrl Pts',(-0.721412305161677,-1.93101141539988,
0.362522932653306));
#16394=CARTESIAN_POINT('Ctrl Pts',(-1.2255735069054,-1.52604510705262,0.32548561922047));
#16395=CARTESIAN_POINT('Ctrl Pts',(-1.67757250343746,-1.1629779682701,0.29228031018839));
#16396=CARTESIAN_POINT('Ctrl Pts',(-1.95230952873461,-0.579091046852653,
0.25907500115631));
#16397=CARTESIAN_POINT('Ctrl Pts',(-1.95633598837559,0.00127248296362327,
0.22586969212423));
#16398=CARTESIAN_POINT('Ctrl Pts',(-1.95588590413641,0.00206796222160181,
0.124130307875766));
#16399=CARTESIAN_POINT('Ctrl Pts',(-1.95149442603296,-0.570486119123227,
0.156904012808695));
#16400=CARTESIAN_POINT('Ctrl Pts',(-1.68517377795595,-1.14821417361252,
0.189677717741624));
#16401=CARTESIAN_POINT('Ctrl Pts',(-1.24335992644724,-1.51202006337354,
0.222451422674553));
#16402=CARTESIAN_POINT('Ctrl Pts',(-0.74355823061328,-1.92357529197494,
0.259526659786979));
#16403=CARTESIAN_POINT('Ctrl Pts',(-0.0191734218330693,-2.06136888910912,
0.296601896899404));
#16404=CARTESIAN_POINT('Ctrl Pts',(0.59730918482247,-1.86366268614966,0.33367713401183));
#16405=CARTESIAN_POINT('Ctrl Pts',(1.21379179147801,-1.6659564831902,0.370752371124255));
#16406=CARTESIAN_POINT('Ctrl Pts',(1.72237219600888,-1.13275048013712,0.40782760823668));
#16407=CARTESIAN_POINT('Ctrl Pts',(1.89021021423941,-0.507705222320547,
0.444902845349105));
#16408=CARTESIAN_POINT('Ctrl Pts',(2.05804823246995,0.117340035496022,0.481978082461531));
#16409=CARTESIAN_POINT('Ctrl Pts',(1.88514386440015,0.834224548076076,0.519053319573957));
#16410=CARTESIAN_POINT('Ctrl Pts',(1.45061079828058,1.31401352267999,0.556128556686382));
#16411=CARTESIAN_POINT('Ctrl Pts',(1.01607773216101,1.7938024972839,0.593203793798808));
#16412=CARTESIAN_POINT('Ctrl Pts',(0.319915967991662,2.03649593391168,0.630279030911233));
#16413=CARTESIAN_POINT('Ctrl Pts',(-0.318741968595543,1.93105881108975,
0.667354268023658));
#16414=CARTESIAN_POINT('Ctrl Pts',(-0.95739990518275,1.82562168826782,0.704429505136084));
#16415=CARTESIAN_POINT('Ctrl Pts',(-1.53855401418781,1.37205400599619,0.74150474224851));
#16416=CARTESIAN_POINT('Ctrl Pts',(-1.79588703923712,0.778131328327298,
0.778579979360935));
#16417=CARTESIAN_POINT('Ctrl Pts',(-1.9012727786294,0.534901837996683,0.793763422199212));
#16418=CARTESIAN_POINT('Ctrl Pts',(-1.95234877280959,0.268132669686638,
0.808946865037489));
#16419=CARTESIAN_POINT('Ctrl Pts',(-1.95120671878141,0.000942122514504899,
0.824130307875766));
#16420=CARTESIAN_POINT('Origin',(0.,0.,0.));
#16421=CARTESIAN_POINT('',(-1.95279514498571,-0.00168107824419284,1.62586969212423));
#16422=CARTESIAN_POINT('',(-1.95278388634516,-0.00168888116712579,1.52413030787576));
#16423=CARTESIAN_POINT('',(-1.954,-2.39295984553393E-16,0.));
#16424=CARTESIAN_POINT('Ctrl Pts',(-1.95279514498571,-0.00168107824419284,
1.62586969212423));
#16425=CARTESIAN_POINT('Ctrl Pts',(-1.94903681723145,0.45580829851081,1.59981878225084));
#16426=CARTESIAN_POINT('Ctrl Pts',(-1.78858836662353,0.915672122197071,
1.57376787237745));
#16427=CARTESIAN_POINT('Ctrl Pts',(-1.49506049969948,1.26310357403151,1.54771696250405));
#16428=CARTESIAN_POINT('Ctrl Pts',(-1.07774365121422,1.75705666974124,1.51067964907122));
#16429=CARTESIAN_POINT('Ctrl Pts',(-0.391431901374392,2.02374896425016,
1.47364233563838));
#16430=CARTESIAN_POINT('Ctrl Pts',(0.249914641927464,1.94117972705521,1.43660502220554));
#16431=CARTESIAN_POINT('Ctrl Pts',(0.891261185229321,1.85861048986026,1.39956770877271));
#16432=CARTESIAN_POINT('Ctrl Pts',(1.48764252199321,1.42677972096142,1.36253039533987));
#16433=CARTESIAN_POINT('Ctrl Pts',(1.76623794405498,0.843232102738223,1.32549308190704));
#16434=CARTESIAN_POINT('Ctrl Pts',(2.04483336611675,0.25968448451502,1.2884557684742));
#16435=CARTESIAN_POINT('Ctrl Pts',(2.0056428734764,-0.475579983032552,1.25141845504136));
#16436=CARTESIAN_POINT('Ctrl Pts',(1.66659475578394,-1.02620605156362,1.21438114160853));
#16437=CARTESIAN_POINT('Ctrl Pts',(1.32754663809148,-1.57683212009468,1.17734382817569));
#16438=CARTESIAN_POINT('Ctrl Pts',(0.688640895346918,-1.94281978960923,
1.14030651474286));
#16439=CARTESIAN_POINT('Ctrl Pts',(0.0421509461412053,-1.956746580861,1.10326920131002));
#16440=CARTESIAN_POINT('Ctrl Pts',(-0.604339003064511,-1.97067337211277,
1.06623188787719));
#16441=CARTESIAN_POINT('Ctrl Pts',(-1.25841315873137,-1.63253928510176,
1.02919457444435));
#16442=CARTESIAN_POINT('Ctrl Pts',(-1.62085801283843,-1.09702287625329,
0.992157261011514));
#16443=CARTESIAN_POINT('Ctrl Pts',(-1.83708669330173,-0.777542532858632,
0.970061404715753));
#16444=CARTESIAN_POINT('Ctrl Pts',(-1.94952098456712,-0.38781143817112,
0.947965548419991));
#16445=CARTESIAN_POINT('Ctrl Pts',(-1.95128265771456,0.000979968443958618,
0.92586969212423));
#16446=CARTESIAN_POINT('Ctrl Pts',(-1.95120671878141,0.000942122514504899,
0.824130307875766));
#16447=CARTESIAN_POINT('Ctrl Pts',(-1.94956008223784,-0.384298600093132,
0.846022102149914));
#16448=CARTESIAN_POINT('Ctrl Pts',(-1.83936019485534,-0.770415304222176,
0.867913896424062));
#16449=CARTESIAN_POINT('Ctrl Pts',(-1.62687654459384,-1.08811501975669,
0.889805690698211));
#16450=CARTESIAN_POINT('Ctrl Pts',(-1.26702108380771,-1.62616101710563,
0.926880927810636));
#16451=CARTESIAN_POINT('Ctrl Pts',(-0.613798221141896,-1.96797533873735,
0.963956164923062));
#16452=CARTESIAN_POINT('Ctrl Pts',(0.0333981997247413,-1.95692658607738,
1.00103140203549));
#16453=CARTESIAN_POINT('Ctrl Pts',(0.680594620591375,-1.94587783341741,
1.03810663914791));
#16454=CARTESIAN_POINT('Ctrl Pts',(1.32176459965883,-1.58196600646575,1.07518187626034));
#16455=CARTESIAN_POINT('Ctrl Pts',(1.66305355512094,-1.03196363523784,1.11225711337276));
#16456=CARTESIAN_POINT('Ctrl Pts',(2.00434251058304,-0.481961264009935,
1.14933235048519));
#16457=CARTESIAN_POINT('Ctrl Pts',(2.04575044243979,0.254131651494222,1.18640758759761));
#16458=CARTESIAN_POINT('Ctrl Pts',(1.76829659796069,0.838942597907999,1.22348282471004));
#16459=CARTESIAN_POINT('Ctrl Pts',(1.49084275348159,1.42375354432178,1.26055806182247));
#16460=CARTESIAN_POINT('Ctrl Pts',(0.894527132666635,1.85728252164517,1.29763329893489));
#16461=CARTESIAN_POINT('Ctrl Pts',(0.252653428905354,1.94083943808002,1.33470853604732));
#16462=CARTESIAN_POINT('Ctrl Pts',(-0.389220274855925,2.02439635451486,
1.37178377315974));
#16463=CARTESIAN_POINT('Ctrl Pts',(-1.07665206156353,1.75798121006115,1.40885901027217));
#16464=CARTESIAN_POINT('Ctrl Pts',(-1.49458024744687,1.26369474377317,1.44593424738459));
#16465=CARTESIAN_POINT('Ctrl Pts',(-1.78840024024692,0.916191869184958,
1.47199960088165));
#16466=CARTESIAN_POINT('Ctrl Pts',(-1.94901418738241,0.456060303888852,
1.49806495437871));
#16467=CARTESIAN_POINT('Ctrl Pts',(-1.95278388634516,-0.00168888116712579,
1.52413030787576));
#16468=CARTESIAN_POINT('Origin',(0.,0.,0.));
#16469=CARTESIAN_POINT('',(-1.95720013100772,4.01036975386895E-5,2.32586969212423));
#16470=CARTESIAN_POINT('',(-1.95721475873132,-4.18937055542429E-5,2.22413030787576));
#16471=CARTESIAN_POINT('',(-1.954,-2.39295984553393E-16,0.));
#16472=CARTESIAN_POINT('Ctrl Pts',(-1.95720013100772,4.01036975387313E-5,
2.32586969212423));
#16473=CARTESIAN_POINT('Ctrl Pts',(-1.95720078041499,0.00218844021348119,
2.32574664294735));
#16474=CARTESIAN_POINT('Ctrl Pts',(-1.95719754885173,0.00433677471760079,
2.32562359377048));
#16475=CARTESIAN_POINT('Ctrl Pts',(-1.95719043044659,0.00648509634279326,
2.3255005445936));
#16476=CARTESIAN_POINT('Ctrl Pts',(-1.9550478187754,0.653121371426419,2.28846323116077));
#16477=CARTESIAN_POINT('Ctrl Pts',(-1.60076274017474,1.2985908336322,2.25142591772793));
#16478=CARTESIAN_POINT('Ctrl Pts',(-1.05640644317236,1.64761702679965,2.2143886042951));
#16479=CARTESIAN_POINT('Ctrl Pts',(-0.512050146169983,1.9966432199671,2.17735129086226));
#16480=CARTESIAN_POINT('Ctrl Pts',(0.22237736923411,2.04922614409623,2.14031397742942));
#16481=CARTESIAN_POINT('Ctrl Pts',(0.810904901655155,1.78131122209933,2.10327666399659));
#16482=CARTESIAN_POINT('Ctrl Pts',(1.3994324340762,1.51339630010242,2.06623935056375));
#16483=CARTESIAN_POINT('Ctrl Pts',(1.8420599835142,0.924983531979483,2.02920203713092));
#16484=CARTESIAN_POINT('Ctrl Pts',(1.9363031541186,0.285248202840816,1.99216472369808));
#16485=CARTESIAN_POINT('Ctrl Pts',(2.030546324723,-0.354487126297849,1.95512741026525));
#16486=CARTESIAN_POINT('Ctrl Pts',(1.7764051164938,-1.04554501645225,1.91809009683241));
#16487=CARTESIAN_POINT('Ctrl Pts',(1.29013896790468,-1.47179410874122,1.88105278339957));
#16488=CARTESIAN_POINT('Ctrl Pts',(0.80387281931556,-1.8980432010302,1.84401546996674));
#16489=CARTESIAN_POINT('Ctrl Pts',(0.0854817303665232,-2.05948349545377,
1.8069781565339));
#16490=CARTESIAN_POINT('Ctrl Pts',(-0.536399128085272,-1.88226256360254,
1.76994084310107));
#16491=CARTESIAN_POINT('Ctrl Pts',(-1.15827998653706,-1.70504163175131,
1.73290352966823));
#16492=CARTESIAN_POINT('Ctrl Pts',(-1.68365061449161,-1.18915947362529,
1.69586621623539));
#16493=CARTESIAN_POINT('Ctrl Pts',(-1.87217495490353,-0.570611446107024,
1.65882890280256));
#16494=CARTESIAN_POINT('Ctrl Pts',(-1.92809705865707,-0.387131122580406,
1.64784249924311));
#16495=CARTESIAN_POINT('Ctrl Pts',(-1.95438013781773,-0.194617253664394,
1.63685609568367));
#16496=CARTESIAN_POINT('Ctrl Pts',(-1.95279514498571,-0.00168107824419272,
1.62586969212423));
#16497=CARTESIAN_POINT('Ctrl Pts',(-1.95278388634516,-0.00168888116712579,
1.52413030787576));
#16498=CARTESIAN_POINT('Ctrl Pts',(-1.95437618958592,-0.19503999965723,
1.53514019149113));
#16499=CARTESIAN_POINT('Ctrl Pts',(-1.92798468468382,-0.387966059069047,
1.5461500751065));
#16500=CARTESIAN_POINT('Ctrl Pts',(-1.87182792927594,-0.571799497056349,
1.55715995872187));
#16501=CARTESIAN_POINT('Ctrl Pts',(-1.68272284016263,-1.19084948347563,
1.5942351958343));
#16502=CARTESIAN_POINT('Ctrl Pts',(-1.15608807687694,-1.70679166819193,
1.63131043294672));
#16503=CARTESIAN_POINT('Ctrl Pts',(-0.533290099975553,-1.88316099335306,
1.66838567005915));
#16504=CARTESIAN_POINT('Ctrl Pts',(0.0895078769258353,-2.05953031851418,
1.70546090717157));
#16505=CARTESIAN_POINT('Ctrl Pts',(0.808469067442917,-1.89632678412012,
1.742536144284));
#16506=CARTESIAN_POINT('Ctrl Pts',(1.2940806434107,-1.46834921584087,1.77961138139642));
#16507=CARTESIAN_POINT('Ctrl Pts',(1.77969221937849,-1.04037164756162,1.81668661850885));
#16508=CARTESIAN_POINT('Ctrl Pts',(2.03195418079698,-0.347620045397172,
1.85376185562127));
#16509=CARTESIAN_POINT('Ctrl Pts',(1.93525024356178,0.292404819142093,1.8908370927337));
#16510=CARTESIAN_POINT('Ctrl Pts',(1.83854630632657,0.932429683681362,1.92791232984612));
#16511=CARTESIAN_POINT('Ctrl Pts',(1.39287647043767,1.51972781059545,1.96498756695855));
#16512=CARTESIAN_POINT('Ctrl Pts',(0.802499325163421,1.78512991495868,2.00206280407098));
#16513=CARTESIAN_POINT('Ctrl Pts',(0.212122179889179,2.05053201932191,2.0391380411834));
#16514=CARTESIAN_POINT('Ctrl Pts',(-0.522962274770398,1.99403810113428,
2.07621327829583));
#16515=CARTESIAN_POINT('Ctrl Pts',(-1.06585153299182,1.64154030157863,2.11328851540825));
#16516=CARTESIAN_POINT('Ctrl Pts',(-1.60686689507973,1.29025922210662,2.15023577956409));
#16517=CARTESIAN_POINT('Ctrl Pts',(-1.95701157491646,0.645014173540876,
2.18718304371993));
#16518=CARTESIAN_POINT('Ctrl Pts',(-1.95721475873132,-4.18937055542428E-5,
2.22413030787576));
#16519=CARTESIAN_POINT('Origin',(0.,0.,0.));
#16520=CARTESIAN_POINT('',(-1.95267861104158,0.0016552724044671,3.02586969212423));
#16521=CARTESIAN_POINT('',(-1.95290774954615,0.00171310729769101,2.92413030787577));
#16522=CARTESIAN_POINT('',(-1.954,-2.39295984553393E-16,0.));
#16523=CARTESIAN_POINT('Ctrl Pts',(-1.95267861104158,0.0016552724044671,
3.02586969212423));
#16524=CARTESIAN_POINT('Ctrl Pts',(-1.95426730228936,0.198943040570848,
3.01463719021104));
#16525=CARTESIAN_POINT('Ctrl Pts',(-1.92676912869608,0.39579823972063,3.00340468829784));
#16526=CARTESIAN_POINT('Ctrl Pts',(-1.8683524720406,0.583005555161783,2.99217218638465));
#16527=CARTESIAN_POINT('Ctrl Pts',(-1.67573322844129,1.20029065090429,2.95513487295181));
#16528=CARTESIAN_POINT('Ctrl Pts',(-1.14695545989861,1.71267996796991,2.91809755951898));
#16529=CARTESIAN_POINT('Ctrl Pts',(-0.523913838219462,1.88577589531095,
2.88106024608614));
#16530=CARTESIAN_POINT('Ctrl Pts',(0.0991277834596942,2.05887182265199,
2.84402293265331));
#16531=CARTESIAN_POINT('Ctrl Pts',(0.816433258275323,1.89267436026844,2.80698561922047));
#16532=CARTESIAN_POINT('Ctrl Pts',(1.29986403215874,1.463212197494,2.76994830578763));
#16533=CARTESIAN_POINT('Ctrl Pts',(1.78329480604215,1.03375003471956,2.7329109923548));
#16534=CARTESIAN_POINT('Ctrl Pts',(2.03285087899336,0.341023171554252,2.69587367892196));
#16535=CARTESIAN_POINT('Ctrl Pts',(1.93437033276029,-0.298073569575231,
2.65883636548913));
#16536=CARTESIAN_POINT('Ctrl Pts',(1.83588978652722,-0.93717031070472,2.62179905205629));
#16537=CARTESIAN_POINT('Ctrl Pts',(1.38937262110987,-1.52263692979838,2.58476173862346));
#16538=CARTESIAN_POINT('Ctrl Pts',(0.799082573852251,-1.7866458736405,2.54772442519062));
#16539=CARTESIAN_POINT('Ctrl Pts',(0.208792526594628,-2.05065481748262,
2.51068711175778));
#16540=CARTESIAN_POINT('Ctrl Pts',(-0.525270402503268,-1.99320608607321,
2.47364979832495));
#16541=CARTESIAN_POINT('Ctrl Pts',(-1.06730179468137,-1.64058017638776,
2.43661248489211));
#16542=CARTESIAN_POINT('Ctrl Pts',(-1.60753239434872,-1.28912579681371,
2.39969822063615));
#16543=CARTESIAN_POINT('Ctrl Pts',(-1.95700531140595,-0.644452316926743,
2.36278395638019));
#16544=CARTESIAN_POINT('Ctrl Pts',(-1.95720013100772,4.01036975386895E-5,
2.32586969212423));
#16545=CARTESIAN_POINT('Ctrl Pts',(-1.95721475873132,-4.18937055544587E-5,
2.22413030787576));
#16546=CARTESIAN_POINT('Ctrl Pts',(-1.95721546249205,-0.00227615201876484,
2.22425828083235));
#16547=CARTESIAN_POINT('Ctrl Pts',(-1.9572119680126,-0.00451040806477065,
2.22438625378894));
#16548=CARTESIAN_POINT('Ctrl Pts',(-1.95720426868303,-0.00674464962048316,
2.22451422674553));
#16549=CARTESIAN_POINT('Ctrl Pts',(-1.95497368436953,-0.654030120340289,
2.26158946385795));
#16550=CARTESIAN_POINT('Ctrl Pts',(-1.59981845395926,-1.30009938085624,
2.29866470097038));
#16551=CARTESIAN_POINT('Ctrl Pts',(-1.0545126575596,-1.64884719787949,2.33573993808281));
#16552=CARTESIAN_POINT('Ctrl Pts',(-0.509206861159936,-1.99759501490274,
2.37281517519523));
#16553=CARTESIAN_POINT('Ctrl Pts',(0.226249501229124,-2.04902138843328,
2.40989041230765));
#16554=CARTESIAN_POINT('Ctrl Pts',(0.81478345819529,-1.77955667339696,2.44696564942008));
#16555=CARTESIAN_POINT('Ctrl Pts',(1.40331741516146,-1.51009195836063,2.4840408865325));
#16556=CARTESIAN_POINT('Ctrl Pts',(1.84492896670473,-0.919736154757425,
2.52111612364493));
#16557=CARTESIAN_POINT('Ctrl Pts',(1.93721953774244,-0.279060025103992,
2.55819136075736));
#16558=CARTESIAN_POINT('Ctrl Pts',(2.02951010878015,0.361616104549433,2.59526659786978));
#16559=CARTESIAN_POINT('Ctrl Pts',(1.7724796993123,1.05261256025308,2.63234183498221));
#16560=CARTESIAN_POINT('Ctrl Pts',(1.28393000274363,1.47723315072179,2.66941707209463));
#16561=CARTESIAN_POINT('Ctrl Pts',(0.795380306174951,1.9018537411905,2.70649230920706));
#16562=CARTESIAN_POINT('Ctrl Pts',(0.0753113225054439,2.06009846642426,
2.74356754631949));
#16563=CARTESIAN_POINT('Ctrl Pts',(-0.546256289304822,1.87944090130045,
2.78064278343191));
#16564=CARTESIAN_POINT('Ctrl Pts',(-1.16782390111508,1.69878333617665,2.81771802054433));
#16565=CARTESIAN_POINT('Ctrl Pts',(-1.6908901410661,1.17922348069528,2.85479325765676));
#16566=CARTESIAN_POINT('Ctrl Pts',(-1.875724275851,0.558885028961709,2.89186849476918));
#16567=CARTESIAN_POINT('Ctrl Pts',(-1.92933673865706,0.37895142411412,2.90262243247138));
#16568=CARTESIAN_POINT('Ctrl Pts',(-1.95449266845916,0.190538998342851,
2.91337637017357));
#16569=CARTESIAN_POINT('Ctrl Pts',(-1.95290774954615,0.00171310729769108,
2.92413030787576));
#16570=CARTESIAN_POINT('Origin',(0.,0.,0.));
#16571=CARTESIAN_POINT('',(-1.95135045472565,-0.00103665430809308,3.72586969212423));
#16572=CARTESIAN_POINT('',(-1.95115009645722,-0.000862413589311458,3.62413030787577));
#16573=CARTESIAN_POINT('',(-1.954,-2.39295984553393E-16,0.));
#16574=CARTESIAN_POINT('Ctrl Pts',(-1.95135045472565,-0.00103665430809308,
3.72586969212423));
#16575=CARTESIAN_POINT('Ctrl Pts',(-1.94945762145185,0.39205003232945,3.70352773747472));
#16576=CARTESIAN_POINT('Ctrl Pts',(-1.83432541049109,0.786156754205215,
3.6811857828252));
#16577=CARTESIAN_POINT('Ctrl Pts',(-1.61355237927334,1.1077387582254,3.65884382817569));
#16578=CARTESIAN_POINT('Ctrl Pts',(-1.2475664983152,1.64084043460512,3.62180651474286));
#16579=CARTESIAN_POINT('Ctrl Pts',(-0.591266345378013,1.97463505701166,
3.58476920131002));
#16580=CARTESIAN_POINT('Ctrl Pts',(0.0551170192794968,1.95642494139715,
3.54773188787719));
#16581=CARTESIAN_POINT('Ctrl Pts',(0.701500383937021,1.93821482578265,3.51069457444435));
#16582=CARTESIAN_POINT('Ctrl Pts',(1.33796696031487,1.56799997214707,3.47365726101151));
#16583=CARTESIAN_POINT('Ctrl Pts',(1.67335875584854,1.01513886309221,3.43661994757868));
#16584=CARTESIAN_POINT('Ctrl Pts',(2.00875055138221,0.46227775403734,3.39958263414584));
#16585=CARTESIAN_POINT('Ctrl Pts',(2.04306756607169,-0.273229610436822,
3.36254532071301));
#16586=CARTESIAN_POINT('Ctrl Pts',(1.76061113877997,-0.854918040011614,
3.32550800728017));
#16587=CARTESIAN_POINT('Ctrl Pts',(1.47815471148825,-1.4366064695864,3.28847069384734));
#16588=CARTESIAN_POINT('Ctrl Pts',(0.878924842215338,-1.86447596426182,
3.2514333804145));
#16589=CARTESIAN_POINT('Ctrl Pts',(0.237045219929842,-1.94279335001325,
3.21439606698166));
#16590=CARTESIAN_POINT('Ctrl Pts',(-0.404834402355659,-2.02111073576468,
3.17735875354883));
#16591=CARTESIAN_POINT('Ctrl Pts',(-1.08936377765374,-1.74987601259212,
3.14032144011599));
#16592=CARTESIAN_POINT('Ctrl Pts',(-1.50339810597481,-1.25316821379613,
3.10328412668316));
#16593=CARTESIAN_POINT('Ctrl Pts',(-1.79186605396357,-0.907099615934405,
3.07747931516352));
#16594=CARTESIAN_POINT('Ctrl Pts',(-1.94902885620257,-0.451580677342798,
3.05167450364387));
#16595=CARTESIAN_POINT('Ctrl Pts',(-1.95267861104158,0.0016552724044671,
3.02586969212423));
#16596=CARTESIAN_POINT('Ctrl Pts',(-1.95290774954615,0.00171310729769101,
2.92413030787577));
#16597=CARTESIAN_POINT('Ctrl Pts',(-1.94902850769025,-0.460456467442357,
2.950451607286));
#16598=CARTESIAN_POINT('Ctrl Pts',(-1.78495210853218,-0.925103000270984,
2.97677290669623));
#16599=CARTESIAN_POINT('Ctrl Pts',(-1.48583543343396,-1.27396510910143,
3.00309420610646));
#16600=CARTESIAN_POINT('Ctrl Pts',(-1.06451042661324,-1.76535974744522,
3.04016944321889));
#16601=CARTESIAN_POINT('Ctrl Pts',(-0.375258383353002,-2.02703197614702,
3.07724468033131));
#16602=CARTESIAN_POINT('Ctrl Pts',(0.266023999143107,-1.93905267245523,
3.11431991744374));
#16603=CARTESIAN_POINT('Ctrl Pts',(0.907306381639212,-1.85107336876345,
3.15139515455616));
#16604=CARTESIAN_POINT('Ctrl Pts',(1.50061910337119,-1.4134425326781,3.18847039166859));
#16605=CARTESIAN_POINT('Ctrl Pts',(1.77403619606301,-0.826734304146555,
3.22554562878102));
#16606=CARTESIAN_POINT('Ctrl Pts',(2.04745328875484,-0.240026075615009,
3.26262086589344));
#16607=CARTESIAN_POINT('Ctrl Pts',(2.0009747524065,0.495759545362725,3.29969610300586));
#16608=CARTESIAN_POINT('Ctrl Pts',(1.65590254220004,1.04339867994717,3.33677134011829));
#16609=CARTESIAN_POINT('Ctrl Pts',(1.31083033199357,1.59103781453161,3.37384657723071));
#16610=CARTESIAN_POINT('Ctrl Pts',(0.667164447928974,1.95053046272276,3.41092181434314));
#16611=CARTESIAN_POINT('Ctrl Pts',(0.0199086246964731,1.9571146316129,3.44799705145557));
#16612=CARTESIAN_POINT('Ctrl Pts',(-0.627347198536033,1.96369880050304,
3.485072288568));
#16613=CARTESIAN_POINT('Ctrl Pts',(-1.27819296093644,1.61737449009216,3.52214752568042));
#16614=CARTESIAN_POINT('Ctrl Pts',(-1.63433425949862,1.07686840552899,3.55922276279284));
#16615=CARTESIAN_POINT('Ctrl Pts',(-1.8421662177247,0.761447423909083,3.58085861115382));
#16616=CARTESIAN_POINT('Ctrl Pts',(-1.94963677903995,0.379897976317775,
3.60249445951479));
#16617=CARTESIAN_POINT('Ctrl Pts',(-1.95115009645722,-0.000862413589311458,
3.62413030787577));
#16618=CARTESIAN_POINT('Origin',(0.,0.,0.));
#16619=CARTESIAN_POINT('',(-1.95645463735042,-0.00107680116258307,4.42586969212423));
#16620=CARTESIAN_POINT('',(-1.9560689354221,-0.00131000797615835,4.32413030787576));
#16621=CARTESIAN_POINT('',(-1.954,-2.39295984553393E-16,0.));
#16622=CARTESIAN_POINT('Ctrl Pts',(-1.95645463735042,-0.00107680116258307,
4.42586969212423));
#16623=CARTESIAN_POINT('Ctrl Pts',(-1.95257837355362,0.583548870363389,
4.3924182847384));
#16624=CARTESIAN_POINT('Ctrl Pts',(-1.67319437992126,1.17138871222795,4.35896687735257));
#16625=CARTESIAN_POINT('Ctrl Pts',(-1.21542355114692,1.53407367113183,4.32551546996674));
#16626=CARTESIAN_POINT('Ctrl Pts',(-0.70858085032514,1.93563753794803,4.2884781565339));
#16627=CARTESIAN_POINT('Ctrl Pts',(0.0169438143861521,2.0611871352921,4.25144084310107));
#16628=CARTESIAN_POINT('Ctrl Pts',(0.629251938590984,1.85328854601076,4.21440352966823));
#16629=CARTESIAN_POINT('Ctrl Pts',(1.24156006279581,1.64538995672942,4.1773662162354));
#16630=CARTESIAN_POINT('Ctrl Pts',(1.74065164649418,1.10404318082267,4.14032890280256));
#16631=CARTESIAN_POINT('Ctrl Pts',(1.89821225955213,0.476892707953959,4.10329158936972));
#16632=CARTESIAN_POINT('Ctrl Pts',(2.05577287261007,-0.15025776491475,4.06625427593688));
#16633=CARTESIAN_POINT('Ctrl Pts',(1.87180251502759,-0.86321193474541,4.02921696250405));
#16634=CARTESIAN_POINT('Ctrl Pts',(1.4304602644841,-1.33582179532369,3.99217964907122));
#16635=CARTESIAN_POINT('Ctrl Pts',(0.989118013940611,-1.80843165590198,
3.95514233563838));
#16636=CARTESIAN_POINT('Ctrl Pts',(0.290403870436121,-2.04069720722789,
3.91810502220554));
#16637=CARTESIAN_POINT('Ctrl Pts',(-0.346048402169674,-1.92636625294191,
3.88106770877271));
#16638=CARTESIAN_POINT('Ctrl Pts',(-0.982500674775478,-1.81203529865592,
3.84403039533987));
#16639=CARTESIAN_POINT('Ctrl Pts',(-1.55669107648259,-1.35110783875803,
3.80699308190704));
#16640=CARTESIAN_POINT('Ctrl Pts',(-1.80595047284659,-0.754439743632632,
3.7699557684742));
#16641=CARTESIAN_POINT('Ctrl Pts',(-1.9048495538052,-0.517698713581134,
3.75526040969088));
#16642=CARTESIAN_POINT('Ctrl Pts',(-1.95259546056833,-0.259588333590661,
3.74056505090755));
#16643=CARTESIAN_POINT('Ctrl Pts',(-1.95135045472565,-0.00103665430809308,
3.72586969212423));
#16644=CARTESIAN_POINT('Ctrl Pts',(-1.95115009645722,-0.000862413589311458,
3.62413030787577));
#16645=CARTESIAN_POINT('Ctrl Pts',(-1.95223000307885,-0.272573861314833,
3.63956969662722));
#16646=CARTESIAN_POINT('Ctrl Pts',(-1.89935350538763,-0.543883498707529,
3.65500908537867));
#16647=CARTESIAN_POINT('Ctrl Pts',(-1.79048714938831,-0.790474416076489,
3.67044847413012));
#16648=CARTESIAN_POINT('Ctrl Pts',(-1.52906190599187,-1.38262329440335,
3.70752371124255));
#16649=CARTESIAN_POINT('Ctrl Pts',(-0.944774584475045,-1.83223319234163,
3.74459894835497));
#16650=CARTESIAN_POINT('Ctrl Pts',(-0.305414648672952,-1.93323974896447,
3.7816741854674));
#16651=CARTESIAN_POINT('Ctrl Pts',(0.333945287129141,-2.0342463055873,3.81874942257982));
#16652=CARTESIAN_POINT('Ctrl Pts',(1.0283778372165,-1.7866495208947,3.85582465969225));
#16653=CARTESIAN_POINT('Ctrl Pts',(1.45961198421181,-1.30392748653653,3.89289989680467));
#16654=CARTESIAN_POINT('Ctrl Pts',(1.89084613120712,-0.821205452178361,
3.9299751339171));
#16655=CARTESIAN_POINT('Ctrl Pts',(2.05888187511037,-0.103358168154617,
3.96705037102952));
#16656=CARTESIAN_POINT('Ctrl Pts',(1.88670539052006,0.520611951436678,4.00412560814195));
#16657=CARTESIAN_POINT('Ctrl Pts',(1.71452890592974,1.14458207102797,4.04120084525437));
#16658=CARTESIAN_POINT('Ctrl Pts',(1.20214019284586,1.67467502618682,4.0782760823668));
#16659=CARTESIAN_POINT('Ctrl Pts',(0.58437628040953,1.8679396129137,4.11535131947923));
#16660=CARTESIAN_POINT('Ctrl Pts',(-0.0333876320267997,2.06120419964058,
4.15242655659165));
#16661=CARTESIAN_POINT('Ctrl Pts',(-0.756526743815583,1.9176404179355,4.18950179370408));
#16662=CARTESIAN_POINT('Ctrl Pts',(-1.25361330032381,1.50304614961146,4.2265770308165));
#16663=CARTESIAN_POINT('Ctrl Pts',(-1.68959543059256,1.13941593283223,4.25909478983626));
#16664=CARTESIAN_POINT('Ctrl Pts',(-1.95168429546986,0.567292711935832,
4.29161254885601));
#16665=CARTESIAN_POINT('Ctrl Pts',(-1.9560689354221,-0.00131000797615835,
4.32413030787576));
#16666=CARTESIAN_POINT('Origin',(0.,0.,0.));
#16667=CARTESIAN_POINT('',(-1.95458552907139,0.00173412683576277,5.12586969212423));
#16668=CARTESIAN_POINT('',(-1.9552206747184,0.00161939276430114,5.02413030787577));
#16669=CARTESIAN_POINT('',(-1.954,-2.39295984553393E-16,0.));
#16670=CARTESIAN_POINT('Ctrl Pts',(-1.95458552907139,0.00173412683576277,
5.12586969212423));
#16671=CARTESIAN_POINT('Ctrl Pts',(-1.95579889273049,0.133549336413818,
5.11834614543492));
#16672=CARTESIAN_POINT('Ctrl Pts',(-1.94360248016884,0.265141296927549,
5.11082259874561));
#16673=CARTESIAN_POINT('Ctrl Pts',(-1.91717253101555,0.393809524200435,
5.10329905205629));
#16674=CARTESIAN_POINT('Ctrl Pts',(-1.78706177989932,1.02722427646379,5.06626173862345));
#16675=CARTESIAN_POINT('Ctrl Pts',(-1.31200866513269,1.58978387278703,5.02922442519062));
#16676=CARTESIAN_POINT('Ctrl Pts',(-0.709330998225857,1.82413979092323,
4.99218711175778));
#16677=CARTESIAN_POINT('Ctrl Pts',(-0.106653331319023,2.05849570905944,
4.95514979832495));
#16678=CARTESIAN_POINT('Ctrl Pts',(0.623648887728016,1.96464794900861,4.91811248489211));
#16679=CARTESIAN_POINT('Ctrl Pts',(1.14749162443816,1.58552811433593,4.88107517145928));
#16680=CARTESIAN_POINT('Ctrl Pts',(1.67133436114829,1.20640827966324,4.84403785802644));
#16681=CARTESIAN_POINT('Ctrl Pts',(1.98871761552153,0.542016370368706,4.8070005445936));
#16682=CARTESIAN_POINT('Ctrl Pts',(1.95445124244436,-0.103714902901561,
4.76996323116077));
#16683=CARTESIAN_POINT('Ctrl Pts',(1.9201848693672,-0.749446176171828,4.73292591772793));
#16684=CARTESIAN_POINT('Ctrl Pts',(1.53426886883963,-1.37651681341782,4.6958886042951));
#16685=CARTESIAN_POINT('Ctrl Pts',(0.973244372713117,-1.69806708597997,
4.65885129086226));
#16686=CARTESIAN_POINT('Ctrl Pts',(0.412219876586598,-2.01961735854213,
4.62181397742943));
#16687=CARTESIAN_POINT('Ctrl Pts',(-0.323913115138867,-2.03564726642044,
4.58477666399659));
#16688=CARTESIAN_POINT('Ctrl Pts',(-0.898403214163087,-1.7388237693533,
4.54773935056375));
#16689=CARTESIAN_POINT('Ctrl Pts',(-1.4728933131873,-1.44200027228616,4.51070203713092));
#16690=CARTESIAN_POINT('Ctrl Pts',(-1.88574051951028,-0.832323370273586,
4.47366472369808));
#16691=CARTESIAN_POINT('Ctrl Pts',(-1.94808375420563,-0.188695851123138,
4.43662741026525));
#16692=CARTESIAN_POINT('Ctrl Pts',(-1.95411974768256,-0.126380645212594,
4.43304150421824));
#16693=CARTESIAN_POINT('Ctrl Pts',(-1.95687016300016,-0.0637471906795113,
4.42945559817124));
#16694=CARTESIAN_POINT('Ctrl Pts',(-1.95645463735042,-0.00107680116258307,
4.42586969212423));
#16695=CARTESIAN_POINT('Ctrl Pts',(-1.9560689354221,-0.00131000797615835,
4.32413030787576));
#16696=CARTESIAN_POINT('Ctrl Pts',(-1.95668345810536,-0.0810016754695383,
4.32868778596844));
#16697=CARTESIAN_POINT('Ctrl Pts',(-1.95223589499426,-0.160624189738801,
4.33324526406111));
#16698=CARTESIAN_POINT('Ctrl Pts',(-1.94249551147141,-0.239593869899598,
4.33780274215378));
#16699=CARTESIAN_POINT('Ctrl Pts',(-1.86325716488311,-0.882014866143589,
4.3748779792662));
#16700=CARTESIAN_POINT('Ctrl Pts',(-1.43374647047883,-1.48123210368856,
4.41195321637863));
#16701=CARTESIAN_POINT('Ctrl Pts',(-0.850815960071711,-1.76261346774659,
4.44902845349105));
#16702=CARTESIAN_POINT('Ctrl Pts',(-0.267885449664584,-2.04399483180463,
4.48610369060348));
#16703=CARTESIAN_POINT('Ctrl Pts',(0.468464876745396,-2.00754032237573,
4.52317892771591));
#16704=CARTESIAN_POINT('Ctrl Pts',(1.02075232548754,-1.66995770146661,4.56025416482833));
#16705=CARTESIAN_POINT('Ctrl Pts',(1.57303977422969,-1.3323750805575,4.59732940194076));
#16706=CARTESIAN_POINT('Ctrl Pts',(1.941264345304,-0.693664348168167,4.63440463905318));
#16707=CARTESIAN_POINT('Ctrl Pts',(1.95666204750888,-0.0465582032952289,
4.67147987616561));
#16708=CARTESIAN_POINT('Ctrl Pts',(1.97205974971376,0.6005479415777,4.70855511327803));
#16709=CARTESIAN_POINT('Ctrl Pts',(1.63463058304921,1.25604949893424,4.74563035039046));
#16710=CARTESIAN_POINT('Ctrl Pts',(1.09902444690466,1.61951823074648,4.78270558750289));
#16711=CARTESIAN_POINT('Ctrl Pts',(0.56341831076011,1.98298696255872,4.81978082461531));
#16712=CARTESIAN_POINT('Ctrl Pts',(-0.170364794864445,2.05442286882665,
4.85685606172773));
#16713=CARTESIAN_POINT('Ctrl Pts',(-0.766018779707725,1.80108557937185,
4.89393129884016));
#16714=CARTESIAN_POINT('Ctrl Pts',(-1.361672764551,1.54774828991705,4.93100653595259));
#16715=CARTESIAN_POINT('Ctrl Pts',(-1.81919762861299,0.96963780473953,4.96808177306502));
#16716=CARTESIAN_POINT('Ctrl Pts',(-1.92890143946537,0.331712632206103,
5.00515701017744));
#16717=CARTESIAN_POINT('Ctrl Pts',(-1.9476151256888,0.222892971156397,5.01148144274355));
#16718=CARTESIAN_POINT('Ctrl Pts',(-1.95620763248682,0.112332773766476,
5.01780587530966));
#16719=CARTESIAN_POINT('Ctrl Pts',(-1.9552206747184,0.00161939276430114,
5.02413030787577));
#16720=CARTESIAN_POINT('Origin',(0.,0.,0.));
#16721=CARTESIAN_POINT('',(-1.95079790389112,-3.269510144494E-5,5.82586969212423));
#16722=CARTESIAN_POINT('',(-1.95085192255358,0.000383174536113729,5.72413030787576));
#16723=CARTESIAN_POINT('',(-1.954,-2.39295984553393E-16,0.));
#16724=CARTESIAN_POINT('Ctrl Pts',(-1.95079807093469,-3.26933958413878E-5,
5.82586969212423));
#16725=CARTESIAN_POINT('Ctrl Pts',(-1.95074883721548,0.328029941286317,
5.8072366926986));
#16726=CARTESIAN_POINT('Ctrl Pts',(-1.87242650231768,0.656114687980161,
5.78860369327296));
#16727=CARTESIAN_POINT('Ctrl Pts',(-1.71596284018057,0.941333347646706,
5.76997069384733));
#16728=CARTESIAN_POINT('Ctrl Pts',(-1.40495581640267,1.50827013831881,5.7329333804145));
#16729=CARTESIAN_POINT('Ctrl Pts',(-0.785207871169114,1.90584052998572,
5.69589606698167));
#16730=CARTESIAN_POINT('Ctrl Pts',(-0.140229809906548,1.95217121547304,
5.65885875354883));
#16731=CARTESIAN_POINT('Ctrl Pts',(0.504748251356019,1.99850190096035,5.62182144011599));
#16732=CARTESIAN_POINT('Ctrl Pts',(1.1749564286476,1.69359288026805,5.58478412668316));
#16733=CARTESIAN_POINT('Ctrl Pts',(1.56380177877164,1.17692822962597,5.54774681325032));
#16734=CARTESIAN_POINT('Ctrl Pts',(1.95264712889569,0.660263578983889,5.51070949981748));
#16735=CARTESIAN_POINT('Ctrl Pts',(2.06012965185219,-0.068156701607988,
5.47367218638465));
#16736=CARTESIAN_POINT('Ctrl Pts',(1.83708014107304,-0.675109688693547,
5.43663487295181));
#16737=CARTESIAN_POINT('Ctrl Pts',(1.61403063029389,-1.2820626757791,5.39959755951898));
#16738=CARTESIAN_POINT('Ctrl Pts',(1.06044908577908,-1.76754836935834,5.36256024608614));
#16739=CARTESIAN_POINT('Ctrl Pts',(0.429577047133733,-1.90947637973667,
5.32552293265331));
#16740=CARTESIAN_POINT('Ctrl Pts',(-0.201294991511623,-2.051404390115,5.28848561922047));
#16741=CARTESIAN_POINT('Ctrl Pts',(-0.909457524287529,-1.84977471729243,
5.25144830578764));
#16742=CARTESIAN_POINT('Ctrl Pts',(-1.37095459694257,-1.39682492677941,
5.2144109923548));
#16743=CARTESIAN_POINT('Ctrl Pts',(-1.73870581031982,-1.03588474984214,
5.18489722561128));
#16744=CARTESIAN_POINT('Ctrl Pts',(-1.94982568195559,-0.515357546731067,
5.15538345886775));
#16745=CARTESIAN_POINT('Ctrl Pts',(-1.95458552907139,0.00173412683576277,
5.12586969212423));
#16746=CARTESIAN_POINT('Ctrl Pts',(-1.9552206747184,0.00161939276430114,
5.02413030787577));
#16747=CARTESIAN_POINT('Ctrl Pts',(-1.95042186547898,-0.536693808344559,
5.05488111242208));
#16748=CARTESIAN_POINT('Ctrl Pts',(-1.71915285367837,-1.07862845650355,
5.0856319169684));
#16749=CARTESIAN_POINT('Ctrl Pts',(-1.32368315644793,-1.44172013107889,
5.11638272151471));
#16750=CARTESIAN_POINT('Ctrl Pts',(-0.846878304935377,-1.87948786194111,
5.15345795862714));
#16751=CARTESIAN_POINT('Ctrl Pts',(-0.131385844267519,-2.0572834637762,
5.19053319573957));
#16752=CARTESIAN_POINT('Ctrl Pts',(0.494871066573067,-1.89361998960963,
5.22760843285199));
#16753=CARTESIAN_POINT('Ctrl Pts',(1.12112797741365,-1.72995651544305,5.26468366996442));
#16754=CARTESIAN_POINT('Ctrl Pts',(1.65814933842698,-1.22483396527481,5.30175890707684));
#16755=CARTESIAN_POINT('Ctrl Pts',(1.85980853758091,-0.609759157741489,
5.33883414418927));
#16756=CARTESIAN_POINT('Ctrl Pts',(2.06146773673485,0.00531564979182955,
5.37590938130169));
#16757=CARTESIAN_POINT('Ctrl Pts',(1.9277647740294,0.730342714690214,5.41298461841412));
#16758=CARTESIAN_POINT('Ctrl Pts',(1.51997812810125,1.23302900604299,5.45005985552654));
#16759=CARTESIAN_POINT('Ctrl Pts',(1.11219148217311,1.73571529739576,5.48713509263897));
#16760=CARTESIAN_POINT('Ctrl Pts',(0.430321153022272,2.01606081520293,5.52421032975139));
#16761=CARTESIAN_POINT('Ctrl Pts',(-0.213119314048168,1.94557811718459,
5.56128556686382));
#16762=CARTESIAN_POINT('Ctrl Pts',(-0.856559781118622,1.87509541916625,
5.59836080397625));
#16763=CARTESIAN_POINT('Ctrl Pts',(-1.46157038610868,1.45378450532239,5.63543604108868));
#16764=CARTESIAN_POINT('Ctrl Pts',(-1.75086384963453,0.874739824296975,
5.6725112782011));
#16765=CARTESIAN_POINT('Ctrl Pts',(-1.88512280557994,0.606009472173862,
5.68971762142599));
#16766=CARTESIAN_POINT('Ctrl Pts',(-1.95138199037298,0.30330611490569,5.70692396465088));
#16767=CARTESIAN_POINT('Ctrl Pts',(-1.95085192255358,0.000383174536113729,
5.72413030787576));
#16768=CARTESIAN_POINT('Origin',(0.,0.,0.));
#16769=CARTESIAN_POINT('',(-1.95467666345581,-0.00169153748172557,6.52586969212423));
#16770=CARTESIAN_POINT('',(-1.95381346134878,-0.0017935399644829,6.42413030787577));
#16771=CARTESIAN_POINT('',(-1.954,-2.39295984553393E-16,0.));
#16772=CARTESIAN_POINT('Ctrl Pts',(-1.95467666345581,-0.00169153748172557,
6.52586969212423));
#16773=CARTESIAN_POINT('Ctrl Pts',(-1.94989845242835,0.519322657074601,
6.49612723996228));
#16774=CARTESIAN_POINT('Ctrl Pts',(-1.7351643372623,1.04378980187726,6.46638478780033));
#16775=CARTESIAN_POINT('Ctrl Pts',(-1.36233982826997,1.40523012754949,6.43664233563838));
#16776=CARTESIAN_POINT('Ctrl Pts',(-0.898073529048792,1.85532007158963,
6.39960502220555));
#16777=CARTESIAN_POINT('Ctrl Pts',(-0.188657797713761,2.05260571068844,
6.36256770877271));
#16778=CARTESIAN_POINT('Ctrl Pts',(0.441334197613014,1.90680041588618,6.32553039533987));
#16779=CARTESIAN_POINT('Ctrl Pts',(1.07132619293978,1.76099512108392,6.28849308190704));
#16780=CARTESIAN_POINT('Ctrl Pts',(1.62189445225829,1.2720988923806,6.2514557684742));
#16781=CARTESIAN_POINT('Ctrl Pts',(1.84119904752624,0.663781270447278,6.21441845504137));
#16782=CARTESIAN_POINT('Ctrl Pts',(2.06050364279419,0.055463648513944,6.17738114160853));
#16783=CARTESIAN_POINT('Ctrl Pts',(1.94854457401157,-0.672275366649399,
6.14034382817569));
#16784=CARTESIAN_POINT('Ctrl Pts',(1.556526550614,-1.18653430832568,6.10330651474286));
#16785=CARTESIAN_POINT('Ctrl Pts',(1.16450852721644,-1.70079325000195,6.06626920131002));
#16786=CARTESIAN_POINT('Ctrl Pts',(0.492431549203928,-2.00157211819116,
6.02923188787718));
#16787=CARTESIAN_POINT('Ctrl Pts',(-0.152249713101387,-1.9512713582857,
5.99219457444435));
#16788=CARTESIAN_POINT('Ctrl Pts',(-0.796930975406703,-1.90097059838025,
5.95515726101152));
#16789=CARTESIAN_POINT('Ctrl Pts',(-1.41421652200483,-1.49959021038012,
5.91811994757868));
#16790=CARTESIAN_POINT('Ctrl Pts',(-1.72172624414277,-0.930748421541415,
5.88108263414585));
#16791=CARTESIAN_POINT('Ctrl Pts',(-1.87453175193852,-0.648083672620247,
5.86267832013864));
#16792=CARTESIAN_POINT('Ctrl Pts',(-1.95084670040156,-0.324068969295429,
5.84427400613143));
#16793=CARTESIAN_POINT('Ctrl Pts',(-1.95079807093469,-3.26933958413878E-5,
5.82586969212423));
#16794=CARTESIAN_POINT('Ctrl Pts',(-1.95085192255358,0.000383174536113729,
5.72413030787576));
#16795=CARTESIAN_POINT('Ctrl Pts',(-1.95023983077328,-0.349414785416059,
5.7439992017633));
#16796=CARTESIAN_POINT('Ctrl Pts',(-1.86056894683247,-0.699505544060014,
5.76386809565083));
#16797=CARTESIAN_POINT('Ctrl Pts',(-1.68370318859703,-0.997916657928721,
5.78373698953837));
#16798=CARTESIAN_POINT('Ctrl Pts',(-1.35367274197203,-1.55475001092207,
5.82081222665079));
#16799=CARTESIAN_POINT('Ctrl Pts',(-0.7200355266604,-1.9316382687018,5.85788746376322));
#16800=CARTESIAN_POINT('Ctrl Pts',(-0.0731991044283191,-1.95584662548515,
5.89496270087565));
#16801=CARTESIAN_POINT('Ctrl Pts',(0.573637317803748,-1.9800549822685,5.93203793798808));
#16802=CARTESIAN_POINT('Ctrl Pts',(1.23367294695625,-1.65158343805548,5.9691131751005));
#16803=CARTESIAN_POINT('Ctrl Pts',(1.60440177887889,-1.12097662310535,6.00618841221292));
#16804=CARTESIAN_POINT('Ctrl Pts',(1.97513061080152,-0.590369808155209,
6.04326364932535));
#16805=CARTESIAN_POINT('Ctrl Pts',(2.05655264549427,0.142372277532039,6.08033888643777));
#16806=CARTESIAN_POINT('Ctrl Pts',(1.81135015364285,0.741420988743503,6.1174141235502));
#16807=CARTESIAN_POINT('Ctrl Pts',(1.56614766179142,1.34046969995497,6.15448936066263));
#16808=CARTESIAN_POINT('Ctrl Pts',(0.994320643395809,1.80582503669066,6.19156459777505));
#16809=CARTESIAN_POINT('Ctrl Pts',(0.357948800551169,1.92420559652088,6.22863983488748));
#16810=CARTESIAN_POINT('Ctrl Pts',(-0.278423042293462,2.04258615635109,
6.2657150719999));
#16811=CARTESIAN_POINT('Ctrl Pts',(-0.97933970958712,1.81399193927586,6.30279030911233));
#16812=CARTESIAN_POINT('Ctrl Pts',(-1.42356034057997,1.34319300038089,6.33986554622475));
#16813=CARTESIAN_POINT('Ctrl Pts',(-1.76010254058954,0.986515035416152,
6.36795380010842));
#16814=CARTESIAN_POINT('Ctrl Pts',(-1.9493114895094,0.49082125388787,6.3960420539921));
#16815=CARTESIAN_POINT('Ctrl Pts',(-1.95381346134878,-0.0017935399644829,
6.42413030787577));
#16816=CARTESIAN_POINT('Origin',(0.,0.,-1.2940562256037));
#16817=CARTESIAN_POINT('',(-1.55603866428123,-0.00134656425434549,6.75594377439631));
#16818=CARTESIAN_POINT('',(-1.55791343064937,0.000503462391539915,6.89405622560371));
#16819=CARTESIAN_POINT('',(-1.5555,-9.09151186476045E-14,-1.2940562256037));
#16820=CARTESIAN_POINT('',(-1.54730100999696,0.15949869736893,7.4445));
#16821=CARTESIAN_POINT('Ctrl Pts',(-1.55603866428123,-0.00134656425434554,
6.7559437743963));
#16822=CARTESIAN_POINT('Ctrl Pts',(-1.55697159855378,-0.103073339358787,
6.76323863566719));
#16823=CARTESIAN_POINT('Ctrl Pts',(-1.50153911503434,-0.720280229157285,
6.80757081037091));
#16824=CARTESIAN_POINT('Ctrl Pts',(-0.676946582872774,-1.70937536089767,
6.88894029850746));
#16825=CARTESIAN_POINT('Ctrl Pts',(1.06890459630572,-1.49565296874813,7.00005223880597));
#16826=CARTESIAN_POINT('Ctrl Pts',(1.83584092749207,0.0856835708872964,
7.11116417910447));
#16827=CARTESIAN_POINT('Ctrl Pts',(0.924965623038614,1.59014055343882,7.22227611940298));
#16828=CARTESIAN_POINT('Ctrl Pts',(-0.835858495286665,1.63675999125994,
7.33338805970149));
#16829=CARTESIAN_POINT('Ctrl Pts',(-1.49427628245053,0.673892957891604,
7.40746268656716));
#16830=CARTESIAN_POINT('Ctrl Pts',(-1.54730100999696,0.159498697368912,
7.4445));
#16831=CARTESIAN_POINT('',(-0.352169241380506,1.51510959188617,7.4445));
#16832=CARTESIAN_POINT('Origin',(0.,0.,7.4445));
#16833=CARTESIAN_POINT('Ctrl Pts',(-1.55791343064937,0.000503462391539858,
6.8940562256037));
#16834=CARTESIAN_POINT('Ctrl Pts',(-1.55587997194015,-0.488621135891717,
6.9292365352861));
#16835=CARTESIAN_POINT('Ctrl Pts',(-1.04365545248604,-1.49691459517969,
7.00149208208092));
#16836=CARTESIAN_POINT('Ctrl Pts',(0.672826183539381,-1.71093187207897,
7.11082286598819));
#16837=CARTESIAN_POINT('Ctrl Pts',(1.80435891657647,-0.361603954366771,
7.22204857732544));
#16838=CARTESIAN_POINT('Ctrl Pts',(1.27791236939833,1.32169962363241,7.33327428866273));
#16839=CARTESIAN_POINT('Ctrl Pts',(0.152038852759137,1.63230677878407,7.40742476288758));
#16840=CARTESIAN_POINT('Ctrl Pts',(-0.352169241380528,1.51510959188617,
7.44450000000001));
#16841=CARTESIAN_POINT('Origin',(0.,0.,-1.2940562256037));
#16842=CARTESIAN_POINT('',(-1.5529510743802,-2.6025883987463E-5,6.0559437743963));
#16843=CARTESIAN_POINT('',(-1.55535150415969,-0.0014277642860383,6.1940562256037));
#16844=CARTESIAN_POINT('',(-1.5555,-9.09151186476045E-14,-1.2940562256037));
#16845=CARTESIAN_POINT('Ctrl Pts',(-1.5529510743802,-2.60258839871949E-5,
6.0559437743963));
#16846=CARTESIAN_POINT('Ctrl Pts',(-1.55298978632273,-0.257978138044578,
6.07434808840351));
#16847=CARTESIAN_POINT('Ctrl Pts',(-1.36998122495718,-1.03498796260698,
6.12978971584355));
#16848=CARTESIAN_POINT('Ctrl Pts',(-0.143008426055117,-1.83280806515592,
6.2222686567164));
#16849=CARTESIAN_POINT('Ctrl Pts',(1.4620310918033,-1.11449456034272,6.33338059701493));
#16850=CARTESIAN_POINT('Ctrl Pts',(1.72940928754233,0.623475815429911,6.44449253731343));
#16851=CARTESIAN_POINT('Ctrl Pts',(0.414554230167772,1.79104708014026,6.55560447761194));
#16852=CARTESIAN_POINT('Ctrl Pts',(-1.16842639544942,1.35082658514471,6.65942155663957));
#16853=CARTESIAN_POINT('Ctrl Pts',(-1.55223492464296,0.413411664830818,
6.72620132223435));
#16854=CARTESIAN_POINT('Ctrl Pts',(-1.55603866428123,-0.00134656425434554,
6.7559437743963));
#16855=CARTESIAN_POINT('Ctrl Pts',(-1.55535150415969,-0.00142776428603842,
6.1940562256037));
#16856=CARTESIAN_POINT('Ctrl Pts',(-1.55649817143771,-0.126898399140172,
6.20304320883246));
#16857=CARTESIAN_POINT('Ctrl Pts',(-1.48522496230459,-0.768704224613979,
6.24910542917363));
#16858=CARTESIAN_POINT('Ctrl Pts',(-0.59667036110871,-1.73952595846347,
6.33224288662724));
#16859=CARTESIAN_POINT('Ctrl Pts',(1.13899278941852,-1.44381691390763,6.44346859796452));
#16860=CARTESIAN_POINT('Ctrl Pts',(1.83065601360088,0.17532136832598,6.5546943093018));
#16861=CARTESIAN_POINT('Ctrl Pts',(0.844193344579619,1.63380261073593,6.66592002063907));
#16862=CARTESIAN_POINT('Ctrl Pts',(-0.915934603694247,1.5945880622222,6.77714573197635));
#16863=CARTESIAN_POINT('Ctrl Pts',(-1.5455164129256,0.568558209121068,6.85319113363123));
#16864=CARTESIAN_POINT('Ctrl Pts',(-1.55802295943751,0.0268493253573782,
6.89216129817368));
#16865=CARTESIAN_POINT('Ctrl Pts',(-1.55791343064937,0.000503462391539858,
6.8940562256037));
#16866=CARTESIAN_POINT('Origin',(0.,0.,-1.2940562256037));
#16867=CARTESIAN_POINT('',(-1.555966115901,0.00138046790836748,5.3559437743963));
#16868=CARTESIAN_POINT('',(-1.55299394346576,0.000305029677950264,5.49405622560371));
#16869=CARTESIAN_POINT('',(-1.5555,-9.09151186476045E-14,-1.2940562256037));
#16870=CARTESIAN_POINT('Ctrl Pts',(-1.555966115901,0.00138046790836748,
5.3559437743963));
#16871=CARTESIAN_POINT('Ctrl Pts',(-1.55217699502656,-0.410255201607083,
5.38545754113982));
#16872=CARTESIAN_POINT('Ctrl Pts',(-1.17320681553292,-1.34462621114732,
5.45200862131617));
#16873=CARTESIAN_POINT('Ctrl Pts',(0.403496653242899,-1.79354886637635,
5.55559701492538));
#16874=CARTESIAN_POINT('Ctrl Pts',(1.72554797232085,-0.634122566945669,
5.66670895522387));
#16875=CARTESIAN_POINT('Ctrl Pts',(1.46886056527041,1.10547479200108,5.77782089552239));
#16876=CARTESIAN_POINT('Ctrl Pts',(-0.131715923640121,1.83365183655613,
5.88893283582089));
#16877=CARTESIAN_POINT('Ctrl Pts',(-1.36662941760285,1.04145067599478,5.9816404621122));
#16878=CARTESIAN_POINT('Ctrl Pts',(-1.55291188141693,0.261131306893961,
6.03731077497067));
#16879=CARTESIAN_POINT('Ctrl Pts',(-1.5529510743802,-2.60258839871949E-5,
6.0559437743963));
#16880=CARTESIAN_POINT('Ctrl Pts',(-1.55299394346576,0.000305029677950229,
5.49405622560371));
#16881=CARTESIAN_POINT('Ctrl Pts',(-1.55250668207154,-0.278154912341265,
5.51392511949124));
#16882=CARTESIAN_POINT('Ctrl Pts',(-1.34792243677793,-1.07688746067556,
5.5708692504912));
#16883=CARTESIAN_POINT('Ctrl Pts',(-0.0687781849042931,-1.83772416168987,
5.66488861860358));
#16884=CARTESIAN_POINT('Ctrl Pts',(1.50750444735784,-1.05327561457109,5.77611432994086));
#16885=CARTESIAN_POINT('Ctrl Pts',(1.70195476716013,0.696642984640571,5.88734004127814));
#16886=CARTESIAN_POINT('Ctrl Pts',(0.336330007005007,1.80799440678846,5.99856575261541));
#16887=CARTESIAN_POINT('Ctrl Pts',(-1.20233240386818,1.30618107352199,6.10080448072394));
#16888=CARTESIAN_POINT('Ctrl Pts',(-1.55176766731418,0.390722855896857,
6.16596797172003));
#16889=CARTESIAN_POINT('Ctrl Pts',(-1.55535150415969,-0.00142776428603842,
6.1940562256037));
#16890=CARTESIAN_POINT('Origin',(0.,0.,-1.2940562256037));
#16891=CARTESIAN_POINT('',(-1.55745403705147,-0.000857197650203868,4.6559437743963));
#16892=CARTESIAN_POINT('',(-1.55647172954169,0.00128913277620515,4.7940562256037));
#16893=CARTESIAN_POINT('',(-1.5555,-9.09151186476045E-14,-1.2940562256037));
#16894=CARTESIAN_POINT('Ctrl Pts',(-1.55745403705147,-0.000857197650203714,
4.6559437743963));
#16895=CARTESIAN_POINT('Ctrl Pts',(-1.55778482013651,-0.0507465481586787,
4.6595296804433));
#16896=CARTESIAN_POINT('Ctrl Pts',(-1.5329809661149,-0.615588902391355,
4.70015289992314));
#16897=CARTESIAN_POINT('Ctrl Pts',(-0.843859631129698,-1.63325682938675,
4.77781343283583));
#16898=CARTESIAN_POINT('Ctrl Pts',(0.914157055608714,-1.59497455450745,
4.88892537313433));
#16899=CARTESIAN_POINT('Ctrl Pts',(1.83579319504673,-0.0974181938582904,
5.00003731343284));
#16900=CARTESIAN_POINT('Ctrl Pts',(1.07782545884778,1.48926801121999,5.11114925373134));
#16901=CARTESIAN_POINT('Ctrl Pts',(-0.666266304296033,1.713393176152,5.22226119402985));
#16902=CARTESIAN_POINT('Ctrl Pts',(-1.49942664147989,0.726761727184559,
5.30385936758484));
#16903=CARTESIAN_POINT('Ctrl Pts',(-1.55693202540547,0.106313199995716,
5.34842022770699));
#16904=CARTESIAN_POINT('Ctrl Pts',(-1.555966115901,0.00138046790836748,
5.3559437743963));
#16905=CARTESIAN_POINT('Ctrl Pts',(-1.55647172954169,0.00128913277620508,
4.7940562256037));
#16906=CARTESIAN_POINT('Ctrl Pts',(-1.55265159250384,-0.427240132487249,
4.82480703015002));
#16907=CARTESIAN_POINT('Ctrl Pts',(-1.14657973682021,-1.37879177584745,
4.89263307180876));
#16908=CARTESIAN_POINT('Ctrl Pts',(0.464983542380115,-1.77925562259896,
4.99753435057992));
#16909=CARTESIAN_POINT('Ctrl Pts',(1.74748619395055,-0.572933012383953,
5.1087600619172));
#16910=CARTESIAN_POINT('Ctrl Pts',(1.42817970701863,1.15856074316792,5.21998577325448));
#16911=CARTESIAN_POINT('Ctrl Pts',(-0.20024807751692,1.82807576816643,5.33121148459175));
#16912=CARTESIAN_POINT('Ctrl Pts',(-1.38701509520349,1.00164745002229,5.4225683020415));
#16913=CARTESIAN_POINT('Ctrl Pts',(-1.55341590891771,0.24144967335499,5.47684988237881));
#16914=CARTESIAN_POINT('Ctrl Pts',(-1.55299394346576,0.000305029677950229,
5.49405622560371));
#16915=CARTESIAN_POINT('Origin',(0.,0.,-1.2940562256037));
#16916=CARTESIAN_POINT('',(-1.55339080467029,-0.000825238370695906,3.9559437743963));
#16917=CARTESIAN_POINT('',(-1.55714699541918,-0.00104284411826,4.0940562256037));
#16918=CARTESIAN_POINT('',(-1.5555,-9.09151186476045E-14,-1.2940562256037));
#16919=CARTESIAN_POINT('Ctrl Pts',(-1.55339080467029,-0.000825238370696021,
3.9559437743963));
#16920=CARTESIAN_POINT('Ctrl Pts',(-1.55438190323133,-0.206647724104582,
3.97063913317962));
#16921=CARTESIAN_POINT('Ctrl Pts',(-1.42057875865067,-0.929976336606789,
4.02237180539578));
#16922=CARTESIAN_POINT('Ctrl Pts',(-0.325039216866852,-1.80941329116195,
4.11114179104478));
#16923=CARTESIAN_POINT('Ctrl Pts',(1.34361459616473,-1.25472178898058,4.22225373134328));
#16924=CARTESIAN_POINT('Ctrl Pts',(1.78296857449566,0.447939743012656,4.3333656716418));
#16925=CARTESIAN_POINT('Ctrl Pts',(0.591048986302979,1.74077225568864,4.44447761194029));
#16926=CARTESIAN_POINT('Ctrl Pts',(-1.08571442614287,1.45061399985919,4.5520036461918));
#16927=CARTESIAN_POINT('Ctrl Pts',(-1.55436830095327,0.464539543423835,
4.62249236701046));
#16928=CARTESIAN_POINT('Ctrl Pts',(-1.55745403705147,-0.000857197650203714,
4.6559437743963));
#16929=CARTESIAN_POINT('Ctrl Pts',(-1.55714699541918,-0.00104284411826003,
4.0940562256037));
#16930=CARTESIAN_POINT('Ctrl Pts',(-1.55763619195644,-0.0644821423710283,
4.09861370369637));
#16931=CARTESIAN_POINT('Ctrl Pts',(-1.52529338404343,-0.643499375005814,
4.14024641890147));
#16932=CARTESIAN_POINT('Ctrl Pts',(-0.799431294618187,-1.65616118233816,
4.21895437121899));
#16933=CARTESIAN_POINT('Ctrl Pts',(0.959104426053338,-1.56910132141185,
4.33018008255627));
#16934=CARTESIAN_POINT('Ctrl Pts',(1.83849028118038,-0.0437463405035559,
4.44140579389354));
#16935=CARTESIAN_POINT('Ctrl Pts',(1.0326493363287,1.52170812080878,4.55263150523082));
#16936=CARTESIAN_POINT('Ctrl Pts',(-0.719755403894915,1.69230978744094,
4.6638572165681));
#16937=CARTESIAN_POINT('Ctrl Pts',(-1.51031879937117,0.693384867678679,
4.74433212335906));
#16938=CARTESIAN_POINT('Ctrl Pts',(-1.55725740651651,0.0894235565985826,
4.78773179303759));
#16939=CARTESIAN_POINT('Ctrl Pts',(-1.55647172954169,0.00128913277620508,
4.7940562256037));
#16940=CARTESIAN_POINT('Origin',(0.,0.,-1.2940562256037));
#16941=CARTESIAN_POINT('',(-1.55444809594431,0.00131769509984214,3.2559437743963));
#16942=CARTESIAN_POINT('',(-1.55323130759427,-0.000686532414708174,3.3940562256037));
#16943=CARTESIAN_POINT('',(-1.5555,-9.09151186476045E-14,-1.2940562256037));
#16944=CARTESIAN_POINT('Ctrl Pts',(-1.55444809594431,0.00131769509984224,
3.2559437743963));
#16945=CARTESIAN_POINT('Ctrl Pts',(-1.55154267442328,-0.359485027434377,
3.28174858591594));
#16946=CARTESIAN_POINT('Ctrl Pts',(-1.24686166172698,-1.24256912580371,
3.34459071086842));
#16947=CARTESIAN_POINT('Ctrl Pts',(0.222653802667342,-1.82484307132901,
3.44447014925373));
#16948=CARTESIAN_POINT('Ctrl Pts',(1.65372145106143,-0.803014516107455,
3.55558208955224));
#16949=CARTESIAN_POINT('Ctrl Pts',(1.57176630825256,0.953508061332994,3.66669402985075));
#16950=CARTESIAN_POINT('Ctrl Pts',(0.0517707715753711,1.83764706567811,
3.77780597014925));
#16951=CARTESIAN_POINT('Ctrl Pts',(-1.30829594910608,1.14591637592306,3.87422255166444));
#16952=CARTESIAN_POINT('Ctrl Pts',(-1.55188399701554,0.312095099942876,
3.93360181974679));
#16953=CARTESIAN_POINT('Ctrl Pts',(-1.55339080467029,-0.000825238370696021,
3.9559437743963));
#16954=CARTESIAN_POINT('Ctrl Pts',(-1.55323130759427,-0.000686532414707983,
3.3940562256037));
#16955=CARTESIAN_POINT('Ctrl Pts',(-1.55409097737417,-0.216984975064148,
3.40949561435515));
#16956=CARTESIAN_POINT('Ctrl Pts',(-1.4109189051218,-0.95160176519996,3.46201024021903));
#16957=CARTESIAN_POINT('Ctrl Pts',(-0.286969261786828,-1.81648256240041,
3.55160010319533));
#16958=CARTESIAN_POINT('Ctrl Pts',(1.37145934362907,-1.22517734450477,3.66282581453261));
#16959=CARTESIAN_POINT('Ctrl Pts',(1.77275862659963,0.489169815626649,3.77405152586988));
#16960=CARTESIAN_POINT('Ctrl Pts',(0.549083125265984,1.75512620009375,3.88527723720716));
#16961=CARTESIAN_POINT('Ctrl Pts',(-1.10713858120128,1.42631885494224,3.99194547045177));
#16962=CARTESIAN_POINT('Ctrl Pts',(-1.5536565617213,0.451598676262059,4.06153846658395));
#16963=CARTESIAN_POINT('Ctrl Pts',(-1.55714699541918,-0.00104284411826003,
4.0940562256037));
#16964=CARTESIAN_POINT('Origin',(0.,0.,-1.2940562256037));
#16965=CARTESIAN_POINT('',(-1.55804749425921,3.19249239839854E-5,2.5559437743963));
#16966=CARTESIAN_POINT('',(-1.55463050379685,0.00136373510819555,2.6940562256037));
#16967=CARTESIAN_POINT('',(-1.5555,-9.09151186476045E-14,-1.2940562256037));
#16968=CARTESIAN_POINT('Ctrl Pts',(-1.55804749425921,3.19249239839832E-5,
2.5559437743963));
#16969=CARTESIAN_POINT('Ctrl Pts',(-1.55789240629065,-0.513022302446059,
2.59285803865226));
#16970=CARTESIAN_POINT('Ctrl Pts',(-1.00056267955874,-1.54112970888597,
2.66680961634105));
#16971=CARTESIAN_POINT('Ctrl Pts',(0.750568915726592,-1.67817557333754,
2.77779850746269));
#16972=CARTESIAN_POINT('Ctrl Pts',(1.81693142975936,-0.279977017554228,
2.8889104477612));
#16973=CARTESIAN_POINT('Ctrl Pts',(1.22094708256035,1.37437810371544,3.0000223880597));
#16974=CARTESIAN_POINT('Ctrl Pts',(-0.492106140687917,1.77128724302598,
3.11113432835821));
#16975=CARTESIAN_POINT('Ctrl Pts',(-1.46164337385231,0.831798954515017,
3.19644145713707));
#16976=CARTESIAN_POINT('Ctrl Pts',(-1.55571278849084,0.158370470628406,
3.2447112724831));
#16977=CARTESIAN_POINT('Ctrl Pts',(-1.55444809594431,0.00131769509984224,
3.2559437743963));
#16978=CARTESIAN_POINT('Ctrl Pts',(-1.55463050379685,0.0013637351081955,
2.6940562256037));
#16979=CARTESIAN_POINT('Ctrl Pts',(-1.55154239698677,-0.366550683268523,
2.72037752501393));
#16980=CARTESIAN_POINT('Ctrl Pts',(-1.23694887232287,-1.2574453593796,2.78377406153659));
#16981=CARTESIAN_POINT('Ctrl Pts',(0.249957593646744,-1.82194441691009,
2.88424583517168));
#16982=CARTESIAN_POINT('Ctrl Pts',(1.6668940398915,-0.776804039943688,2.99547154650895));
#16983=CARTESIAN_POINT('Ctrl Pts',(1.55589501744036,0.980383063583733,3.10669725784622));
#16984=CARTESIAN_POINT('Ctrl Pts',(0.0187062518377651,1.83891553174339,
3.2179229691835));
#16985=CARTESIAN_POINT('Ctrl Pts',(-1.31986995326957,1.12664004660162,3.31370929176933));
#16986=CARTESIAN_POINT('Ctrl Pts',(-1.55202661709144,0.302421341945843,
3.37242037724273));
#16987=CARTESIAN_POINT('Ctrl Pts',(-1.55323130759427,-0.000686532414707983,
3.3940562256037));
#16988=CARTESIAN_POINT('Origin',(0.,0.,-1.2940562256037));
#16989=CARTESIAN_POINT('',(-1.55454086388192,-0.001338238080313,1.8559437743963));
#16990=CARTESIAN_POINT('',(-1.55805913879558,-3.33498767488005E-5,1.9940562256037));
#16991=CARTESIAN_POINT('',(-1.5555,-9.09151186476045E-14,-1.2940562256037));
#16992=CARTESIAN_POINT('Ctrl Pts',(-1.55454086388192,-0.00133823808031298,
1.8559437743963));
#16993=CARTESIAN_POINT('Ctrl Pts',(-1.55580261226994,-0.154926887448841,
1.86693017795574));
#16994=CARTESIAN_POINT('Ctrl Pts',(-1.46434456543453,-0.824823376066396,
1.91495389494802));
#16995=CARTESIAN_POINT('Ctrl Pts',(-0.503833422351614,-1.76798718278107,
2.00001492537314));
#16996=CARTESIAN_POINT('Ctrl Pts',(1.211812440791,-1.38243900779253,2.11112686567164));
#16997=CARTESIAN_POINT('Ctrl Pts',(1.81874690762903,0.2679303086893,2.22223880597015));
#16998=CARTESIAN_POINT('Ctrl Pts',(0.761673489280804,1.67316479305249,2.33335074626865));
#16999=CARTESIAN_POINT('Ctrl Pts',(-0.99227021626331,1.54758740541246,2.44446268656716));
#17000=CARTESIAN_POINT('Ctrl Pts',(-1.5572711215541,0.518216278848874,2.51866036260971));
#17001=CARTESIAN_POINT('Ctrl Pts',(-1.55804801122595,0.00174212832754369,
2.55582072521942));
#17002=CARTESIAN_POINT('Ctrl Pts',(-1.55804749425921,3.19249239839832E-5,
2.5559437743963));
#17003=CARTESIAN_POINT('Ctrl Pts',(-1.55805913879558,-3.33498767486382E-5,
1.9940562256037));
#17004=CARTESIAN_POINT('Ctrl Pts',(-1.5580596990309,-0.00181195213168648,
1.99418419856029));
#17005=CARTESIAN_POINT('Ctrl Pts',(-1.5572509939767,-0.518871555499298,
2.0313874086293));
#17006=CARTESIAN_POINT('Ctrl Pts',(-0.990825815880477,-1.5492657736205,
2.10566585581074));
#17007=CARTESIAN_POINT('Ctrl Pts',(0.765574959497512,-1.6720811124538,2.21689156714802));
#17008=CARTESIAN_POINT('Ctrl Pts',(1.82022199392772,-0.262206313316451,
2.32811727848529));
#17009=CARTESIAN_POINT('Ctrl Pts',(1.20638759997596,1.38801628675575,2.43934298982257));
#17010=CARTESIAN_POINT('Ctrl Pts',(-0.513265374585843,1.76593287340023,
2.55056870115984));
#17011=CARTESIAN_POINT('Ctrl Pts',(-1.46682634638563,0.818764115677731,
2.63547311308689));
#17012=CARTESIAN_POINT('Ctrl Pts',(-1.55589219334096,0.151680354105525,
2.68330228790151));
#17013=CARTESIAN_POINT('Ctrl Pts',(-1.55463050379685,0.0013637351081955,
2.6940562256037));
#17014=CARTESIAN_POINT('Origin',(0.,0.,-1.2940562256037));
#17015=CARTESIAN_POINT('',(-1.55333683422467,0.00078011305757314,1.1559437743963));
#17016=CARTESIAN_POINT('',(-1.55453190133567,-0.00134444967022529,1.2940562256037));
#17017=CARTESIAN_POINT('',(-1.5555,-9.09151186476045E-14,-1.2940562256037));
#17018=CARTESIAN_POINT('Ctrl Pts',(-1.55333683422467,0.000780113057573043,
1.1559437743963));
#17019=CARTESIAN_POINT('Ctrl Pts',(-1.55193443781686,-0.308720927367064,
1.17803963069206));
#17020=CARTESIAN_POINT('Ctrl Pts',(-1.31240187276934,-1.13901289380036,
1.23717280042066));
#17021=CARTESIAN_POINT('Ctrl Pts',(0.0395921340189295,-1.83794780075079,
1.33334328358209));
#17022=CARTESIAN_POINT('Ctrl Pts',(1.56541283438613,-0.96390406493211,1.44445522388059));
#17023=CARTESIAN_POINT('Ctrl Pts',(1.65900671048959,0.792038431388639,1.55556716417911));
#17024=CARTESIAN_POINT('Ctrl Pts',(0.234741865039883,1.82332721494359,1.66667910447761));
#17025=CARTESIAN_POINT('Ctrl Pts',(-1.24223016373737,1.24939407250205,1.76680464121668));
#17026=CARTESIAN_POINT('Ctrl Pts',(-1.55154901187489,0.362850464858491,
1.8298928645229));
#17027=CARTESIAN_POINT('Ctrl Pts',(-1.55454086388192,-0.00133823808031298,
1.8559437743963));
#17028=CARTESIAN_POINT('Ctrl Pts',(-1.55453190133567,-0.00134444967022513,
1.2940562256037));
#17029=CARTESIAN_POINT('Ctrl Pts',(-1.55579946924303,-0.155263418355649,
1.30506610921907));
#17030=CARTESIAN_POINT('Ctrl Pts',(-1.46404280977096,-0.826019057429759,
1.35315122994686));
#17031=CARTESIAN_POINT('Ctrl Pts',(-0.501082205369057,-1.76942810040879,
1.43831158778708));
#17032=CARTESIAN_POINT('Ctrl Pts',(1.21592516185098,-1.37966899434435,1.54953729912436));
#17033=CARTESIAN_POINT('Ctrl Pts',(1.8183716526183,0.274745208061178,1.66076301046163));
#17034=CARTESIAN_POINT('Ctrl Pts',(0.754032712405612,1.67731773070425,1.77198872179891));
#17035=CARTESIAN_POINT('Ctrl Pts',(-0.999460041113845,1.5425554247787,1.8830864601796));
#17036=CARTESIAN_POINT('Ctrl Pts',(-1.5578973924169,0.513469573665662,1.95710896144786));
#17037=CARTESIAN_POINT('Ctrl Pts',(-1.55805913879558,-3.33498767486382E-5,
1.9940562256037));
#17038=CARTESIAN_POINT('Origin',(0.,0.,-1.2940562256037));
#17039=CARTESIAN_POINT('',(-1.55735958542387,0.00101297198046619,0.455943774396298));
#17040=CARTESIAN_POINT('',(-1.55327638232574,0.000749985450956003,0.594056225603703));
#17041=CARTESIAN_POINT('',(-1.5555,-9.09151186476045E-14,-1.2940562256037));
#17042=CARTESIAN_POINT('Ctrl Pts',(-1.55735958542387,0.00101297198046621,
0.455943774396298));
#17043=CARTESIAN_POINT('Ctrl Pts',(-1.55415428451722,-0.460990851268869,
0.489149083428377));
#17044=CARTESIAN_POINT('Ctrl Pts',(-1.09150079880486,-1.44424863810505,
0.559391705893293));
#17045=CARTESIAN_POINT('Ctrl Pts',(0.579516952736672,-1.74455562530747,
0.666671641791043));
#17046=CARTESIAN_POINT('Ctrl Pts',(1.77995215483547,-0.45979539180552,0.777783582089551));
#17047=CARTESIAN_POINT('Ctrl Pts',(1.35190460952174,1.24581651128198,0.888895522388059));
#17048=CARTESIAN_POINT('Ctrl Pts',(-0.313043761712607,1.81151378121076,
1.00000746268657));
#17049=CARTESIAN_POINT('Ctrl Pts',(-1.41743746237044,0.936955068058493,
1.08902354668931));
#17050=CARTESIAN_POINT('Ctrl Pts',(-1.55428514985164,0.21006806585223,1.14100231725922));
#17051=CARTESIAN_POINT('Ctrl Pts',(-1.55333683422467,0.000780113057573043,
1.1559437743963));
#17052=CARTESIAN_POINT('Ctrl Pts',(-1.55327638232574,0.000749985450955847,
0.594056225603703));
#17053=CARTESIAN_POINT('Ctrl Pts',(-1.55196556188379,-0.305924499715954,
0.61594801987785));
#17054=CARTESIAN_POINT('Ctrl Pts',(-1.3156705723219,-1.13385132195631,0.674915051264423));
#17055=CARTESIAN_POINT('Ctrl Pts',(0.0313843551128396,-1.83872969125081,
0.770957319763422));
#17056=CARTESIAN_POINT('Ctrl Pts',(1.56261245507102,-0.969643437172017,
0.882183031100698));
#17057=CARTESIAN_POINT('Ctrl Pts',(1.66150197094076,0.788277540412492,0.993408742437974));
#17058=CARTESIAN_POINT('Ctrl Pts',(0.237394066880885,1.82362194812979,1.10463445377525));
#17059=CARTESIAN_POINT('Ctrl Pts',(-1.24180780125352,1.25035520807598,1.20485028149716));
#17060=CARTESIAN_POINT('Ctrl Pts',(-1.55153099717163,0.363051076099792,
1.26799087210664));
#17061=CARTESIAN_POINT('Ctrl Pts',(-1.55453190133567,-0.00134444967022513,
1.2940562256037));
#17062=CARTESIAN_POINT('Origin',(0.,0.,7.5));
#17063=CARTESIAN_POINT('',(-1.90714972453263,0.000559583190138325,7.09553262944276));
#17064=CARTESIAN_POINT('Ctrl Pts',(-0.352169241380463,1.51510959188618,
7.4445));
#17065=CARTESIAN_POINT('Ctrl Pts',(-0.294581668876612,1.53128067531421,
7.44178679402676));
#17066=CARTESIAN_POINT('Ctrl Pts',(-0.236177221040451,1.54382025621514,
7.43908623010619));
#17067=CARTESIAN_POINT('Ctrl Pts',(-0.17725379571509,1.55288079770358,7.43639376053775));
#17068=CARTESIAN_POINT('Ctrl Pts',(-0.119240420394871,1.56180140255761,
7.43374287514286));
#17069=CARTESIAN_POINT('Ctrl Pts',(-0.0607231436400752,1.56734934022223,
7.4310998360025));
#17070=CARTESIAN_POINT('Ctrl Pts',(-0.00197185718845893,1.56962582506071,
7.42846030289105));
#17071=CARTESIAN_POINT('Ctrl Pts',(0.0296117181373077,1.57084962005681,
7.4270413400413));
#17072=CARTESIAN_POINT('Ctrl Pts',(0.0612630953454002,1.57112724793077,
7.42562339041052));
#17073=CARTESIAN_POINT('Ctrl Pts',(0.0929408476792332,1.57046939552494,
7.42420577971289));
#17074=CARTESIAN_POINT('Ctrl Pts',(0.105200379607973,1.57021480162293,7.42365715355322));
#17075=CARTESIAN_POINT('Ctrl Pts',(0.117460267523568,1.56982005993498,7.42310873898429));
#17076=CARTESIAN_POINT('Ctrl Pts',(0.129708286104984,1.56928654809906,7.42256093565192));
#17077=CARTESIAN_POINT('Ctrl Pts',(0.192428535028528,1.56655451475585,7.41975571771902));
#17078=CARTESIAN_POINT('Ctrl Pts',(0.254912080108278,1.56018641116159,7.41696316059146));
#17079=CARTESIAN_POINT('Ctrl Pts',(0.316835955987319,1.55031158486179,7.41417821827426));
#17080=CARTESIAN_POINT('Ctrl Pts',(0.379261168612821,1.54035681180124,7.41137072901695));
#17081=CARTESIAN_POINT('Ctrl Pts',(0.441118681165113,1.52683817797346,7.40857097836836));
#17082=CARTESIAN_POINT('Ctrl Pts',(0.502077268456636,1.50983552777742,7.40577379678119));
#17083=CARTESIAN_POINT('Ctrl Pts',(0.518104654250298,1.50536514802758,7.40503835473071));
#17084=CARTESIAN_POINT('Ctrl Pts',(0.534069848209942,1.50065364953946,7.40430309027496));
#17085=CARTESIAN_POINT('Ctrl Pts',(0.549966680795085,1.49570190223715,7.40356790945547));
#17086=CARTESIAN_POINT('Ctrl Pts',(0.559908491182372,1.4926051008774,7.40310813054867));
#17087=CARTESIAN_POINT('Ctrl Pts',(0.569821116728089,1.48941503409471,7.4026484967243));
#17088=CARTESIAN_POINT('Ctrl Pts',(0.579694961183896,1.486134869268,7.40218936420725));
#17089=CARTESIAN_POINT('Ctrl Pts',(0.640449229714658,1.46595184779153,7.39936429841276));
#17090=CARTESIAN_POINT('Ctrl Pts',(0.69982505895545,1.44233435228215,7.39655407027566));
#17091=CARTESIAN_POINT('Ctrl Pts',(0.757493396577592,1.41540064986381,7.39375356846506));
#17092=CARTESIAN_POINT('Ctrl Pts',(0.814802366573082,1.38863478825924,7.39097051833992));
#17093=CARTESIAN_POINT('Ctrl Pts',(0.870426121162267,1.35859365369072,7.38819707369729));
#17094=CARTESIAN_POINT('Ctrl Pts',(0.924030095744784,1.32534364884642,7.38542821816778));
#17095=CARTESIAN_POINT('Ctrl Pts',(0.960999915716867,1.30241164235365,7.38351858196539));
#17096=CARTESIAN_POINT('Ctrl Pts',(0.997008764456124,1.27795226352036,7.38161112864094));
#17097=CARTESIAN_POINT('Ctrl Pts',(1.03193962221215,1.25197434532887,7.3797042125328));
#17098=CARTESIAN_POINT('Ctrl Pts',(1.0531065792895,1.23623257674251,7.37854868375383));
#17099=CARTESIAN_POINT('Ctrl Pts',(1.07387756970412,1.21993300461795,7.37739335223873));
#17100=CARTESIAN_POINT('Ctrl Pts',(1.09422502955045,1.2030757852037,7.37623785181303));
#17101=CARTESIAN_POINT('Ctrl Pts',(1.10258166584356,1.19615257942657,7.37576329150589));
#17102=CARTESIAN_POINT('Ctrl Pts',(1.11086633597203,1.18913559341204,7.3752887282991));
#17103=CARTESIAN_POINT('Ctrl Pts',(1.11906690491304,1.18203401934788,7.37481473623418));
#17104=CARTESIAN_POINT('Ctrl Pts',(1.12385025457867,1.17789170773882,7.37453825910173));
#17105=CARTESIAN_POINT('Ctrl Pts',(1.12860592464056,1.17371985114455,7.37426192347451));
#17106=CARTESIAN_POINT('Ctrl Pts',(1.13333360310225,1.16951854601392,7.37398572456616));
#17107=CARTESIAN_POINT('Ctrl Pts',(1.17895537492945,1.12897624060986,7.37132042410681));
#17108=CARTESIAN_POINT('Ctrl Pts',(1.22197272212526,1.08569548753383,7.36866785506909));
#17109=CARTESIAN_POINT('Ctrl Pts',(1.2623504524016,1.0400250384405,7.36602371637222));
#17110=CARTESIAN_POINT('Ctrl Pts',(1.30450707484485,0.992342519733652,7.36326308678831));
#17111=CARTESIAN_POINT('Ctrl Pts',(1.34378698003833,0.942054513171778,7.36051164672689));
#17112=CARTESIAN_POINT('Ctrl Pts',(1.38011608577908,0.889512321374444,7.35776450122604));
#17113=CARTESIAN_POINT('Ctrl Pts',(1.41047885103542,0.845599150293909,7.35546852029652));
#17114=CARTESIAN_POINT('Ctrl Pts',(1.43877996472123,0.800110306074669,7.35317553916464));
#17115=CARTESIAN_POINT('Ctrl Pts',(1.46495451960825,0.753233209535809,7.35088270017959));
#17116=CARTESIAN_POINT('Ctrl Pts',(1.47224608288955,0.740174446270043,7.35024397372845));
#17117=CARTESIAN_POINT('Ctrl Pts',(1.47937249019278,0.727007875170104,7.34960525830843));
#17118=CARTESIAN_POINT('Ctrl Pts',(1.48633203561836,0.713737394565328,7.34896649214163));
#17119=CARTESIAN_POINT('Ctrl Pts',(1.49231636613785,0.702326456460141,7.34841723387359));
#17120=CARTESIAN_POINT('Ctrl Pts',(1.49817791288619,0.690837217360077,7.34786787112171));
#17121=CARTESIAN_POINT('Ctrl Pts',(1.50390644072503,0.679291229674037,7.3473192635151));
#17122=CARTESIAN_POINT('Ctrl Pts',(1.53283760232342,0.620979767295612,7.34454859437159));
#17123=CARTESIAN_POINT('Ctrl Pts',(1.55843652026989,0.561117048195595,7.34179201389979));
#17124=CARTESIAN_POINT('Ctrl Pts',(1.58063784893836,0.500065381838401,7.33904470742869));
#17125=CARTESIAN_POINT('Ctrl Pts',(1.6031119912636,0.438263502347606,7.3362636415941));
#17126=CARTESIAN_POINT('Ctrl Pts',(1.62210502961578,0.375242296860671,7.33349207908152));
#17127=CARTESIAN_POINT('Ctrl Pts',(1.63750518239391,0.311348169568812,7.33072502553951));
#17128=CARTESIAN_POINT('Ctrl Pts',(1.65022992907376,0.258554109936303,7.32843868098962));
#17129=CARTESIAN_POINT('Ctrl Pts',(1.66050103147123,0.20516326683894,7.32615541484386));
#17130=CARTESIAN_POINT('Ctrl Pts',(1.66822949082188,0.151363515297575,7.32387240968315));
#17131=CARTESIAN_POINT('Ctrl Pts',(1.67108031331177,0.13151822211743,7.32303026998087));
#17132=CARTESIAN_POINT('Ctrl Pts',(1.67358492004799,0.111617257557933,7.32218816579018));
#17133=CARTESIAN_POINT('Ctrl Pts',(1.67573795844748,0.091670001678837,7.32134595570008));
#17134=CARTESIAN_POINT('Ctrl Pts',(1.67695445834914,0.0803994944639542,
7.32087009400991));
#17135=CARTESIAN_POINT('Ctrl Pts',(1.67805865914088,0.0691137533863127,
7.3203941797156));
#17136=CARTESIAN_POINT('Ctrl Pts',(1.67904845798992,0.0578298683786967,
7.31991883455417));
#17137=CARTESIAN_POINT('Ctrl Pts',(1.68482856592515,-0.00806440229655341,
7.31714297121365));
#17138=CARTESIAN_POINT('Ctrl Pts',(1.68672581172374,-0.0740201346390124,
7.31438118276366));
#17139=CARTESIAN_POINT('Ctrl Pts',(1.68463949062778,-0.139690992105407,
7.31162863136205));
#17140=CARTESIAN_POINT('Ctrl Pts',(1.68257287237932,-0.204741665606402,
7.30890207456915));
#17141=CARTESIAN_POINT('Ctrl Pts',(1.67659788793627,-0.2695138491763,7.30618458118234));
#17142=CARTESIAN_POINT('Ctrl Pts',(1.6665669476348,-0.3336793478161,7.30347144913232));
#17143=CARTESIAN_POINT('Ctrl Pts',(1.65656393293128,-0.397666213161047,
7.30076587029591));
#17144=CARTESIAN_POINT('Ctrl Pts',(1.64252742158424,-0.461050667219861,
7.29806462854663));
#17145=CARTESIAN_POINT('Ctrl Pts',(1.62468485220914,-0.523589263699737,
7.29536306097687));
#17146=CARTESIAN_POINT('Ctrl Pts',(1.62063291677799,-0.537791386138751,
7.29474955195105));
#17147=CARTESIAN_POINT('Ctrl Pts',(1.61638449230085,-0.551949831001097,
7.29413602612215));
#17148=CARTESIAN_POINT('Ctrl Pts',(1.61194189299792,-0.566061632343824,
7.29352242888019));
#17149=CARTESIAN_POINT('Ctrl Pts',(1.60819661792182,-0.577958401384625,
7.29300514377289));
#17150=CARTESIAN_POINT('Ctrl Pts',(1.60431575784587,-0.589814146380397,
7.2924881495291));
#17151=CARTESIAN_POINT('Ctrl Pts',(1.60030378247776,-0.601620053553602,
7.29197172819479));
#17152=CARTESIAN_POINT('Ctrl Pts',(1.57922949506156,-0.663634661857349,
7.28925904662807));
#17153=CARTESIAN_POINT('Ctrl Pts',(1.55452233752644,-0.724336859414935,
7.28655946062951));
#17154=CARTESIAN_POINT('Ctrl Pts',(1.52646885207918,-0.783492431203164,
7.28386844992972));
#17155=CARTESIAN_POINT('Ctrl Pts',(1.49785765329009,-0.843824036953083,
7.28112394097306));
#17156=CARTESIAN_POINT('Ctrl Pts',(1.46576530908513,-0.902547787676455,
7.27838835166439));
#17157=CARTESIAN_POINT('Ctrl Pts',(1.43044176155356,-0.95940342094092,7.27565688674544));
#17158=CARTESIAN_POINT('Ctrl Pts',(1.40719192683218,-0.996825598744453,
7.27385904614475));
#17159=CARTESIAN_POINT('Ctrl Pts',(1.38254116404519,-1.03343820105651,7.27206299232293));
#17160=CARTESIAN_POINT('Ctrl Pts',(1.35654982896749,-1.06916144614065,7.2702673579332));
#17161=CARTESIAN_POINT('Ctrl Pts',(1.34005703462379,-1.09182962123443,7.26912793863759));
#17162=CARTESIAN_POINT('Ctrl Pts',(1.32302428798857,-1.11413959500617,7.26798868822771));
#17163=CARTESIAN_POINT('Ctrl Pts',(1.30546545072429,-1.13606969941564,7.26684925734159));
#17164=CARTESIAN_POINT('Ctrl Pts',(1.29557863985671,-1.1484178288128,7.26620768082384));
#17165=CARTESIAN_POINT('Ctrl Pts',(1.28552143085819,-1.16064953781435,7.26556582874875));
#17166=CARTESIAN_POINT('Ctrl Pts',(1.27531693894013,-1.17273679271259,7.26492492457875));
#17167=CARTESIAN_POINT('Ctrl Pts',(1.23124484751569,-1.2249403328029,7.26215692913113));
#17168=CARTESIAN_POINT('Ctrl Pts',(1.18437118678711,-1.27452793646465,7.25940270292496));
#17169=CARTESIAN_POINT('Ctrl Pts',(1.1349613540182,-1.32123869434595,7.25665745327404));
#17170=CARTESIAN_POINT('Ctrl Pts',(1.0857776821155,-1.36773564568569,7.25392476930092));
#17171=CARTESIAN_POINT('Ctrl Pts',(1.03408031096501,-1.41138288844598,7.25120097989535));
#17172=CARTESIAN_POINT('Ctrl Pts',(0.980088635865932,-1.45189422149834,
7.24848135788222));
#17173=CARTESIAN_POINT('Ctrl Pts',(0.928612197667789,-1.49051830805181,
7.24588843120928));
#17174=CARTESIAN_POINT('Ctrl Pts',(0.875049469874555,-1.52629233307795,
7.24329929269164));
#17175=CARTESIAN_POINT('Ctrl Pts',(0.819562927233232,-1.55893273310611,
7.24070984551053));
#17176=CARTESIAN_POINT('Ctrl Pts',(0.806531597661789,-1.56659851637287,
7.24010169913812));
#17177=CARTESIAN_POINT('Ctrl Pts',(0.793394057897985,-1.57409127964972,
7.2394935357407));
#17178=CARTESIAN_POINT('Ctrl Pts',(0.78015224431478,-1.58140700410033,7.23888530224817));
#17179=CARTESIAN_POINT('Ctrl Pts',(0.770009447983695,-1.58701060987914,
7.23841941527599));
#17180=CARTESIAN_POINT('Ctrl Pts',(0.759805087672894,-1.59251043302504,
7.23795347189941));
#17181=CARTESIAN_POINT('Ctrl Pts',(0.749553755678445,-1.59789772385032,
7.23748806565584));
#17182=CARTESIAN_POINT('Ctrl Pts',(0.716202490399591,-1.61542451603163,
7.23597393197059));
#17183=CARTESIAN_POINT('Ctrl Pts',(0.682319909404191,-1.63177984026051,
7.23446389597977));
#17184=CARTESIAN_POINT('Ctrl Pts',(0.647945625107734,-1.64691812240344,
7.23295717369848));
#17185=CARTESIAN_POINT('Ctrl Pts',(0.587919642023283,-1.67335329876966,
7.23032606477447));
#17186=CARTESIAN_POINT('Ctrl Pts',(0.52639576498612,-1.69608014520221,7.22770506060276));
#17187=CARTESIAN_POINT('Ctrl Pts',(0.46370862765048,-1.71520377795159,7.22508998649035));
#17188=CARTESIAN_POINT('Ctrl Pts',(0.400150801058184,-1.73459302725791,
7.22243859046197));
#17189=CARTESIAN_POINT('Ctrl Pts',(0.335396320744255,-1.75027834108098,
7.21979329036732));
#17190=CARTESIAN_POINT('Ctrl Pts',(0.269772608446838,-1.76232212244813,
7.21714973513363));
#17191=CARTESIAN_POINT('Ctrl Pts',(0.241062234316718,-1.76759127679625,
7.2159931797189));
#17192=CARTESIAN_POINT('Ctrl Pts',(0.2121852884367,-1.77216281037181,7.21483695828146));
#17193=CARTESIAN_POINT('Ctrl Pts',(0.183168585619119,-1.77603911617646,
7.21368070646147));
#17194=CARTESIAN_POINT('Ctrl Pts',(0.164433789661126,-1.77854187463173,
7.21293416602716));
#17195=CARTESIAN_POINT('Ctrl Pts',(0.145640727943501,-1.78075477785065,
7.21218761292724));
#17196=CARTESIAN_POINT('Ctrl Pts',(0.126796600025785,-1.78267808932064,
7.21144094909238));
#17197=CARTESIAN_POINT('Ctrl Pts',(0.114847127630937,-1.78389770306013,
7.21096747327424));
#17198=CARTESIAN_POINT('Ctrl Pts',(0.102876237812544,-1.78500084411828,
7.21049391856396));
#17199=CARTESIAN_POINT('Ctrl Pts',(0.0909023739078884,-1.78598642534176,
7.21002091434047));
#17200=CARTESIAN_POINT('Ctrl Pts',(0.0223150311249881,-1.79163192104421,
7.20731150465678));
#17201=CARTESIAN_POINT('Ctrl Pts',(-0.0464949765975819,-1.79343822563924,
7.204615131498));
#17202=CARTESIAN_POINT('Ctrl Pts',(-0.115169948787061,-1.79150548386327,
7.201927305065));
#17203=CARTESIAN_POINT('Ctrl Pts',(-0.184810802193317,-1.78954555898233,
7.1992016756161));
#17204=CARTESIAN_POINT('Ctrl Pts',(-0.254313838210283,-1.78374072590431,
7.19648483499498));
#17205=CARTESIAN_POINT('Ctrl Pts',(-0.323317077031426,-1.77414310096439,
7.19377210128489));
#17206=CARTESIAN_POINT('Ctrl Pts',(-0.390207228852162,-1.76483938420678,
7.19114243965136));
#17207=CARTESIAN_POINT('Ctrl Pts',(-0.456628689115353,-1.75197132856033,
7.18851663724823));
#17208=CARTESIAN_POINT('Ctrl Pts',(-0.522247153731527,-1.73553989954365,
7.18589042924469));
#17209=CARTESIAN_POINT('Ctrl Pts',(-0.542667798244601,-1.73042639417967,
7.18507314617701));
#17210=CARTESIAN_POINT('Ctrl Pts',(-0.563010584939934,-1.72496745463069,
7.1842558238281));
#17211=CARTESIAN_POINT('Ctrl Pts',(-0.583265123016525,-1.71916221233715,
7.18343833365983));
#17212=CARTESIAN_POINT('Ctrl Pts',(-0.594324986363522,-1.71599229623144,
7.18299194828612));
#17213=CARTESIAN_POINT('Ctrl Pts',(-0.605348577565269,-1.71272196767285,
7.18254591460309));
#17214=CARTESIAN_POINT('Ctrl Pts',(-0.616333858846904,-1.70935174383982,
7.18210023125036));
#17215=CARTESIAN_POINT('Ctrl Pts',(-0.683725730938223,-1.68867628841438,
7.17936607863924));
#17216=CARTESIAN_POINT('Ctrl Pts',(-0.749681756569652,-1.66424383897131,
7.17664487770965));
#17217=CARTESIAN_POINT('Ctrl Pts',(-0.813838416597903,-1.63611281928401,
7.17393200937892));
#17218=CARTESIAN_POINT('Ctrl Pts',(-0.876849560193779,-1.60848407863208,
7.17126757928126));
#17219=CARTESIAN_POINT('Ctrl Pts',(-0.938126029319885,-1.57728744952324,
7.16861118688198));
#17220=CARTESIAN_POINT('Ctrl Pts',(-0.997312296090875,-1.54253001527406,
7.16595845612799));
#17221=CARTESIAN_POINT('Ctrl Pts',(-1.02347117496609,-1.52716808146505,
7.16478601417029));
#17222=CARTESIAN_POINT('Ctrl Pts',(-1.0492215115725,-1.51110995120918,7.16361428748691));
#17223=CARTESIAN_POINT('Ctrl Pts',(-1.07453112510484,-1.49435330423123,
7.16244289826465));
#17224=CARTESIAN_POINT('Ctrl Pts',(-1.10516814559263,-1.47406955963299,
7.16102494395429));
#17225=CARTESIAN_POINT('Ctrl Pts',(-1.13515946112038,-1.45276234916859,
7.15960748412057));
#17226=CARTESIAN_POINT('Ctrl Pts',(-1.16448435570839,-1.43047866030764,
7.15818984863178));
#17227=CARTESIAN_POINT('Ctrl Pts',(-1.17968931872586,-1.41892456370188,
7.15745480438074));
#17228=CARTESIAN_POINT('Ctrl Pts',(-1.1947150759586,-1.40710789339051,7.15671971290617));
#17229=CARTESIAN_POINT('Ctrl Pts',(-1.20955844125675,-1.39503487170675,
7.15598448079515));
#17230=CARTESIAN_POINT('Ctrl Pts',(-1.2184705964626,-1.38778606788849,7.1555430375945));
#17231=CARTESIAN_POINT('Ctrl Pts',(-1.22730979594949,-1.38045068721632,
7.15510189992037));
#17232=CARTESIAN_POINT('Ctrl Pts',(-1.23607420347025,-1.37303174210186,
7.15466112096385));
#17233=CARTESIAN_POINT('Ctrl Pts',(-1.28876418024182,-1.32843043336258,
7.1520112404185));
#17234=CARTESIAN_POINT('Ctrl Pts',(-1.33877042848354,-1.2807988909053,7.14937346465996));
#17235=CARTESIAN_POINT('Ctrl Pts',(-1.38599825103533,-1.23050256527184,
7.14674359103655));
#17236=CARTESIAN_POINT('Ctrl Pts',(-1.43425343070737,-1.17911213270163,
7.14405650919887));
#17237=CARTESIAN_POINT('Ctrl Pts',(-1.47960859192691,-1.1249390060584,7.14137767702936));
#17238=CARTESIAN_POINT('Ctrl Pts',(-1.52193138288134,-1.06832685423381,
7.13870261160338));
#17239=CARTESIAN_POINT('Ctrl Pts',(-1.55066539724144,-1.02989143098312,
7.13688644195504));
#17240=CARTESIAN_POINT('Ctrl Pts',(-1.57800101601077,-0.990330805152557,
7.13507200854792));
#17241=CARTESIAN_POINT('Ctrl Pts',(-1.60388667803358,-0.949743456777433,
7.13325790847962));
#17242=CARTESIAN_POINT('Ctrl Pts',(-1.62003594041973,-0.924422267854757,
7.13212614766269));
#17243=CARTESIAN_POINT('Ctrl Pts',(-1.63562069179463,-0.898701332888775,
7.13099451658541));
#17244=CARTESIAN_POINT('Ctrl Pts',(-1.65062655993749,-0.872603512387977,
7.12986267459833));
#17245=CARTESIAN_POINT('Ctrl Pts',(-1.65635574489922,-0.862639461036616,
7.12943054151348));
#17246=CARTESIAN_POINT('Ctrl Pts',(-1.66200053139848,-0.852620464599865,
7.12899837768465));
#17247=CARTESIAN_POINT('Ctrl Pts',(-1.66756006049801,-0.842547771324513,
7.12856616415337));
#17248=CARTESIAN_POINT('Ctrl Pts',(-1.67344140782474,-0.831892011347815,
7.12810893156204));
#17249=CARTESIAN_POINT('Ctrl Pts',(-1.67922337730384,-0.821183277061747,
7.1276519494335));
#17250=CARTESIAN_POINT('Ctrl Pts',(-1.68490302697532,-0.810427767612281,
7.1271953846437));
#17251=CARTESIAN_POINT('Ctrl Pts',(-1.71867201689079,-0.746479687863883,
7.12448082781816));
#17252=CARTESIAN_POINT('Ctrl Pts',(-1.74885449180758,-0.680831600304512,
7.12177889893296));
#17253=CARTESIAN_POINT('Ctrl Pts',(-1.77532011389704,-0.613841133314895,
7.11908508207449));
#17254=CARTESIAN_POINT('Ctrl Pts',(-1.80172135822353,-0.547013620983615,
7.11639781793949));
#17255=CARTESIAN_POINT('Ctrl Pts',(-1.82442431805884,-0.478849290745972,
7.11371862641413));
#17256=CARTESIAN_POINT('Ctrl Pts',(-1.84325651205081,-0.409674689769748,
7.11104302445964));
#17257=CARTESIAN_POINT('Ctrl Pts',(-1.86148527154818,-0.34271663033918,
7.10845315603751));
#17258=CARTESIAN_POINT('Ctrl Pts',(-1.87608759212419,-0.274811091848995,
7.10586665083265));
#17259=CARTESIAN_POINT('Ctrl Pts',(-1.88686151657838,-0.206241373327113,
7.1032794430912));
#17260=CARTESIAN_POINT('Ctrl Pts',(-1.8894237591873,-0.189934199908044,
7.10266415625292));
#17261=CARTESIAN_POINT('Ctrl Pts',(-1.89176925852511,-0.173589436851263,
7.10204882968071));
#17262=CARTESIAN_POINT('Ctrl Pts',(-1.89389487850133,-0.157210868172391,
7.10143340868806));
#17263=CARTESIAN_POINT('Ctrl Pts',(-1.89540717923759,-0.145558116622667,
7.10099555919912));
#17264=CARTESIAN_POINT('Ctrl Pts',(-1.89680805540638,-0.133888495556873,
7.10055767143479));
#17265=CARTESIAN_POINT('Ctrl Pts',(-1.89809506960791,-0.12221735851089,
7.10012024866215));
#17266=CARTESIAN_POINT('Ctrl Pts',(-1.90260558085945,-0.0813143172688235,
7.09858724278285));
#17267=CARTESIAN_POINT('Ctrl Pts',(-1.90572389008592,-0.0403491830271802,
7.09705830708501));
#17268=CARTESIAN_POINT('Ctrl Pts',(-1.90742224034152,0.000616434489977578,
7.09553262952215));
#17269=CARTESIAN_POINT('',(0.084982434829279,1.94905960819019,7.046));
#17270=CARTESIAN_POINT('Ctrl Pts',(0.0849160311153282,1.94854955259671,
7.046));
#17271=CARTESIAN_POINT('Ctrl Pts',(0.0133469932817959,1.94202022424704,
7.05556311378236));
#17272=CARTESIAN_POINT('Ctrl Pts',(-0.057643443386169,1.9317481562341,7.06516697216295));
#17273=CARTESIAN_POINT('Ctrl Pts',(-0.127716536696194,1.91775362299336,
7.07483035053949));
#17274=CARTESIAN_POINT('Ctrl Pts',(-0.195999508457667,1.90411660095032,
7.08424686352096));
#17275=CARTESIAN_POINT('Ctrl Pts',(-0.263412231749455,1.88694439734026,
7.09371989428859));
#17276=CARTESIAN_POINT('Ctrl Pts',(-0.329616946053496,1.86621372408347,
7.10326681575032));
#17277=CARTESIAN_POINT('Ctrl Pts',(-0.373950818831073,1.85233146448275,
7.10965989524551));
#17278=CARTESIAN_POINT('Ctrl Pts',(-0.41774246810674,1.83685263442241,7.11608610945697));
#17279=CARTESIAN_POINT('Ctrl Pts',(-0.460881457798893,1.81976080684648,
7.12255067528795));
#17280=CARTESIAN_POINT('Ctrl Pts',(-0.497884301533585,1.80510014303758,
7.12809571287374));
#17281=CARTESIAN_POINT('Ctrl Pts',(-0.53440686918178,1.7892525808674,7.13366896766314));
#17282=CARTESIAN_POINT('Ctrl Pts',(-0.570374125039445,1.77220369526276,
7.13927373202269));
#17283=CARTESIAN_POINT('Ctrl Pts',(-0.580625413497348,1.76734446872319,
7.14087118656344));
#17284=CARTESIAN_POINT('Ctrl Pts',(-0.590829427779041,1.7623885644236,7.14247087519816));
#17285=CARTESIAN_POINT('Ctrl Pts',(-0.600974912742468,1.75734066833771,
7.14407135449713));
#17286=CARTESIAN_POINT('Ctrl Pts',(-0.660532286239387,1.72770783820246,
7.15346670067592));
#17287=CARTESIAN_POINT('Ctrl Pts',(-0.718171394717493,1.69486290257124,
7.16290421661148));
#17288=CARTESIAN_POINT('Ctrl Pts',(-0.77359140837187,1.65879255638639,7.17240215454285));
#17289=CARTESIAN_POINT('Ctrl Pts',(-0.79145555504589,1.64716560228914,7.17546373004814));
#17290=CARTESIAN_POINT('Ctrl Pts',(-0.809088855973432,1.63520322368412,
7.17853158362642));
#17291=CARTESIAN_POINT('Ctrl Pts',(-0.826480388876073,1.62290416848565,
7.18160632658995));
#17292=CARTESIAN_POINT('Ctrl Pts',(-0.88415727734301,1.5821158585131,7.19180333498275));
#17293=CARTESIAN_POINT('Ctrl Pts',(-0.93917932864386,1.5376265413157,7.20207611531283));
#17294=CARTESIAN_POINT('Ctrl Pts',(-0.99133911172057,1.48977648468554,7.21244696501856));
#17295=CARTESIAN_POINT('Ctrl Pts',(-1.03697892191269,1.44790768513415,7.22152145851107));
#17296=CARTESIAN_POINT('Ctrl Pts',(-1.0804266997828,1.40346470822021,7.2306710363693));
#17297=CARTESIAN_POINT('Ctrl Pts',(-1.12150612234599,1.35666626833897,7.23991063613496));
#17298=CARTESIAN_POINT('Ctrl Pts',(-1.12930267296081,1.34778429331443,7.24166423934404));
#17299=CARTESIAN_POINT('Ctrl Pts',(-1.13701438607344,1.338816634524,7.24342123717376));
#17300=CARTESIAN_POINT('Ctrl Pts',(-1.14462934985433,1.32977774514085,7.24517924126443));
#17301=CARTESIAN_POINT('Ctrl Pts',(-1.18689780114357,1.27960549657953,7.25493741115345));
#17302=CARTESIAN_POINT('Ctrl Pts',(-1.22626964349749,1.22715044372182,7.26474446593405));
#17303=CARTESIAN_POINT('Ctrl Pts',(-1.2626041554744,1.17270468062558,7.27462138727731));
#17304=CARTESIAN_POINT('Ctrl Pts',(-1.29870272792618,1.11861246314731,7.28443417245898));
#17305=CARTESIAN_POINT('Ctrl Pts',(-1.33180351900955,1.06255418531111,7.29431591978697));
#17306=CARTESIAN_POINT('Ctrl Pts',(-1.36171904589852,1.00480435475497,7.30428720484495));
#17307=CARTESIAN_POINT('Ctrl Pts',(-1.39100085763464,0.948277866941019,
7.31404726332289));
#17308=CARTESIAN_POINT('Ctrl Pts',(-1.41723097430462,0.890129769006774,
7.32389310626744));
#17309=CARTESIAN_POINT('Ctrl Pts',(-1.44018415693848,0.83062133555421,7.33384402917814));
#17310=CARTESIAN_POINT('Ctrl Pts',(-1.44632047771148,0.814712307068312,
7.33650431624776));
#17311=CARTESIAN_POINT('Ctrl Pts',(-1.45222231211246,0.798706119319694,
7.33917211349499));
#17312=CARTESIAN_POINT('Ctrl Pts',(-1.45788473508532,0.78260794455952,7.34184778960142));
#17313=CARTESIAN_POINT('Ctrl Pts',(-1.46140114941093,0.772610836852428,
7.34350940792919));
#17314=CARTESIAN_POINT('Ctrl Pts',(-1.4648248277114,0.762579164108622,7.34517391187186));
#17315=CARTESIAN_POINT('Ctrl Pts',(-1.46815093425694,0.752525994362274,
7.34683944075502));
#17316=CARTESIAN_POINT('Ctrl Pts',(-1.4875809575628,0.693798674658319,7.35656891411169));
#17317=CARTESIAN_POINT('Ctrl Pts',(-1.50372373374688,0.634230525264841,
7.36635120065226));
#17318=CARTESIAN_POINT('Ctrl Pts',(-1.51642546703182,0.574066612526935,
7.37620769393241));
#17319=CARTESIAN_POINT('Ctrl Pts',(-1.52890893161854,0.514936566476241,
7.385894811592));
#17320=CARTESIAN_POINT('Ctrl Pts',(-1.53806859003218,0.455230176794947,
7.39565360754218));
#17321=CARTESIAN_POINT('Ctrl Pts',(-1.54370934814325,0.395188284726392,
7.40550439129109));
#17322=CARTESIAN_POINT('Ctrl Pts',(-1.54918565956382,0.33689681170573,7.41506799222619));
#17323=CARTESIAN_POINT('Ctrl Pts',(-1.55134510253712,0.278288450517533,
7.42471829564676));
#17324=CARTESIAN_POINT('Ctrl Pts',(-1.54996382900015,0.219602494440036,
7.43447388607445));
#17325=CARTESIAN_POINT('Ctrl Pts',(-1.54949240817649,0.199573310494113,
7.43780341375428));
#17326=CARTESIAN_POINT('Ctrl Pts',(-1.5486081708139,0.179535297751125,7.44114520545616));
#17327=CARTESIAN_POINT('Ctrl Pts',(-1.54730100999696,0.159498697368912,
7.4445));
#17328=CARTESIAN_POINT('',(-1.49051052577446,1.26051379553366,7.046));
#17329=CARTESIAN_POINT('Origin',(0.,0.,7.046));
#17330=CARTESIAN_POINT('Ctrl Pts',(-1.90742224034152,0.000616434489977578,
7.09553262952215));
#17331=CARTESIAN_POINT('Ctrl Pts',(-1.90876164805009,0.0329240599094907,
7.09432940051696));
#17332=CARTESIAN_POINT('Ctrl Pts',(-1.90921779267002,0.0652320529994964,
7.09312819770054));
#17333=CARTESIAN_POINT('Ctrl Pts',(-1.90877477964874,0.0975109530601205,
7.09192862283081));
#17334=CARTESIAN_POINT('Ctrl Pts',(-1.90781024899833,0.16778877103618,7.08931690111213));
#17335=CARTESIAN_POINT('Ctrl Pts',(-1.90258719753853,0.237928585345474,
7.08671289622934));
#17336=CARTESIAN_POINT('Ctrl Pts',(-1.89333689480301,0.307653748465392,
7.08411249814515));
#17337=CARTESIAN_POINT('Ctrl Pts',(-1.88389965579861,0.378787964046921,
7.0814595494873));
#17338=CARTESIAN_POINT('Ctrl Pts',(-1.87027048866354,0.449491484193812,
7.0788103548782));
#17339=CARTESIAN_POINT('Ctrl Pts',(-1.8526408196263,0.519466411196971,7.0761605500361));
#17340=CARTESIAN_POINT('Ctrl Pts',(-1.84839799409914,0.536306852496432,
7.07552283757523));
#17341=CARTESIAN_POINT('Ctrl Pts',(-1.8439232315986,0.553105040705889,7.07488508977019));
#17342=CARTESIAN_POINT('Ctrl Pts',(-1.83921877202327,0.569856697426902,
7.07424724578707));
#17343=CARTESIAN_POINT('Ctrl Pts',(-1.83514299244073,0.584369748149054,
7.07369464002192));
#17344=CARTESIAN_POINT('Ctrl Pts',(-1.83089368872409,0.598851100707912,
7.07314183740804));
#17345=CARTESIAN_POINT('Ctrl Pts',(-1.82648012174354,0.613273349358239,
7.07258974257699));
#17346=CARTESIAN_POINT('Ctrl Pts',(-1.80525925753629,0.682616939592868,
7.06993521631944));
#17347=CARTESIAN_POINT('Ctrl Pts',(-1.78021580797096,0.750706522102631,
7.06729279368472));
#17348=CARTESIAN_POINT('Ctrl Pts',(-1.75159954554489,0.817253861437449,
7.06465826007958));
#17349=CARTESIAN_POINT('Ctrl Pts',(-1.72257788914062,0.884743947600279,
7.06198640419794));
#17350=CARTESIAN_POINT('Ctrl Pts',(-1.68988110151814,0.950648721336099,
7.05932266244995));
#17351=CARTESIAN_POINT('Ctrl Pts',(-1.65371662519363,1.01465825897231,7.05666263857406));
#17352=CARTESIAN_POINT('Ctrl Pts',(-1.61767133058481,1.07845685019671,7.05401138093072));
#17353=CARTESIAN_POINT('Ctrl Pts',(-1.57818065931587,1.14037360389397,7.051363816695));
#17354=CARTESIAN_POINT('Ctrl Pts',(-1.53540446982221,1.20007853919048,7.04871559292653));
#17355=CARTESIAN_POINT('Ctrl Pts',(-1.52078518671176,1.2204834271088,7.04781053023934));
#17356=CARTESIAN_POINT('Ctrl Pts',(-1.50578179227618,1.24062970905854,7.04690539051781));
#17357=CARTESIAN_POINT('Ctrl Pts',(-1.49039960333531,1.26050328917698,7.046));
#17358=CARTESIAN_POINT('',(-1.,-1.22464679914735E-16,8.));
#17359=CARTESIAN_POINT('',(-1.5,-1.83697019872103E-16,7.5));
#17360=CARTESIAN_POINT('Origin',(0.,0.,8.));
#17361=CARTESIAN_POINT('Ctrl Pts',(1.13509973994373,-1.59049193030951,-0.230074082272067));
#17362=CARTESIAN_POINT('Ctrl Pts',(1.66385265555159,-1.21313239420412,-0.193036768839232));
#17363=CARTESIAN_POINT('Ctrl Pts',(2.30633309595034,0.10379526882931,-0.11896214197356));
#17364=CARTESIAN_POINT('Ctrl Pts',(1.1618831159781,1.99754257541113,-0.00785020167505245));
#17365=CARTESIAN_POINT('Ctrl Pts',(-1.04657265959996,2.05782619857144,0.103261738623455));
#17366=CARTESIAN_POINT('Ctrl Pts',(-2.29698513032901,0.238308494988224,
0.214373678921962));
#17367=CARTESIAN_POINT('Ctrl Pts',(-1.44610949780919,-1.80077244555215,
0.32548561922047));
#17368=CARTESIAN_POINT('Ctrl Pts',(0.727982080133343,-2.19148935509534,
0.436597559518978));
#17369=CARTESIAN_POINT('Ctrl Pts',(2.23595404085407,-0.577589325353924,
0.547709499817485));
#17370=CARTESIAN_POINT('Ctrl Pts',(1.69824597043106,1.56497940407905,0.658821440115993));
#17371=CARTESIAN_POINT('Ctrl Pts',(-0.393241729595879,2.27560136836119,
0.7699333804145));
#17372=CARTESIAN_POINT('Ctrl Pts',(-2.12493397204,0.90429099396703,0.881045320713008));
#17373=CARTESIAN_POINT('Ctrl Pts',(-1.91248731439823,-1.29440519809075,
0.992157261011514));
#17374=CARTESIAN_POINT('Ctrl Pts',(0.0497351526023427,-2.30880745912378,
1.10326920131002));
#17375=CARTESIAN_POINT('Ctrl Pts',(1.96645238083605,-1.21084445058012,1.21438114160853));
#17376=CARTESIAN_POINT('Ctrl Pts',(2.0840238587571,0.994948952062592,1.32549308190704));
#17377=CARTESIAN_POINT('Ctrl Pts',(0.294879848465431,2.29044125875909,1.43660502220554));
#17378=CARTESIAN_POINT('Ctrl Pts',(-1.76405540105404,1.49036437523231,1.54771696250405));
#17379=CARTESIAN_POINT('Ctrl Pts',(-2.20902124244616,-0.673277315499274,
1.65882890280256));
#17380=CARTESIAN_POINT('Ctrl Pts',(-0.63290935858251,-2.22092378987733,
1.76994084310107));
#17381=CARTESIAN_POINT('Ctrl Pts',(1.5222639082646,-1.73660290660664,1.88105278339957));
#17382=CARTESIAN_POINT('Ctrl Pts',(2.28468753295219,0.336570763856544,1.99216472369808));
#17383=CARTESIAN_POINT('Ctrl Pts',(0.956804884638204,2.10180906822536,2.10327666399659));
#17384=CARTESIAN_POINT('Ctrl Pts',(-1.24647766157407,1.94406029583798,2.2143886042951));
#17385=CARTESIAN_POINT('Ctrl Pts',(-2.30933289737607,0.00765190922063762,
2.3255005445936));
#17386=CARTESIAN_POINT('Ctrl Pts',(-1.25933333160116,-1.9357573546638,2.43661248489211));
#17387=CARTESIAN_POINT('Ctrl Pts',(0.942855455692524,-2.10810354889204,
2.54772442519062));
#17388=CARTESIAN_POINT('Ctrl Pts',(2.28240695194457,-0.35170369161106,2.65883636548913));
#17389=CARTESIAN_POINT('Ctrl Pts',(1.53373873309094,1.72647689788489,2.76994830578763));
#17390=CARTESIAN_POINT('Ctrl Pts',(-0.618177691355928,2.22506928503553,
2.88106024608615));
#17391=CARTESIAN_POINT('Ctrl Pts',(-2.20451099698397,0.687901333838673,
2.99217218638465));
#17392=CARTESIAN_POINT('Ctrl Pts',(-1.77389315295183,-1.47864128941955,
3.10328412668316));
#17393=CARTESIAN_POINT('Ctrl Pts',(0.279694972942425,-2.29234545893725,
3.21439606698166));
#17394=CARTESIAN_POINT('Ctrl Pts',(2.07738458076118,-1.00873697491097,3.32550800728017));
#17395=CARTESIAN_POINT('Ctrl Pts',(1.97443353669272,1.1977851185115,3.43661994757868));
#17396=CARTESIAN_POINT('Ctrl Pts',(0.0650338075591902,2.30842967941821,
3.54773188787719));
#17397=CARTESIAN_POINT('Ctrl Pts',(-1.90386665125239,1.30704581219857,3.65884382817569));
#17398=CARTESIAN_POINT('Ctrl Pts',(-2.13088147818969,-0.890180378860142,
3.7699557684742));
#17399=CARTESIAN_POINT('Ctrl Pts',(-0.408310273068383,-2.2729627585538,
3.88106770877271));
#17400=CARTESIAN_POINT('Ctrl Pts',(1.6878321574451,-1.57616610457607,3.99217964907122));
#17401=CARTESIAN_POINT('Ctrl Pts',(2.23974323019256,0.562696404915903,4.10329158936972));
#17402=CARTESIAN_POINT('Ctrl Pts',(0.742468479097436,2.18673673263618,4.21440352966824));
#17403=CARTESIAN_POINT('Ctrl Pts',(-1.43410551503643,1.81008794060395,4.32551546996673));
#17404=CARTESIAN_POINT('Ctrl Pts',(-2.29858772583325,-0.222646468261011,
4.43662741026525));
#17405=CARTESIAN_POINT('Ctrl Pts',(-1.06004610686433,-2.05167717429874,
4.54773935056375));
#17406=CARTESIAN_POINT('Ctrl Pts',(1.14835286831205,-2.00358745066383,4.65885129086226));
#17407=CARTESIAN_POINT('Ctrl Pts',(2.30610086989477,-0.122375538925838,
4.76996323116077));
#17408=CARTESIAN_POINT('Ctrl Pts',(1.35395110677505,1.87080018895779,4.88107517145928));
#17409=CARTESIAN_POINT('Ctrl Pts',(-0.836955550366062,2.15234346911026,
4.99218711175778));
#17410=CARTESIAN_POINT('Ctrl Pts',(-2.26211489466594,0.464664680140549,
5.10329905205629));
#17411=CARTESIAN_POINT('Ctrl Pts',(-1.61762005706343,-1.64814504446985,
5.2144109923548));
#17412=CARTESIAN_POINT('Ctrl Pts',(0.506867541264277,-2.25303406293758,
5.3255229326533));
#17413=CARTESIAN_POINT('Ctrl Pts',(2.16761217480869,-0.796576982199858,
5.43663487295182));
#17414=CARTESIAN_POINT('Ctrl Pts',(1.84516460593919,1.38868385957575,5.54774681325032));
#17415=CARTESIAN_POINT('Ctrl Pts',(-0.165459925935554,2.30341092165264,
5.65885875354883));
#17416=CARTESIAN_POINT('Ctrl Pts',(-2.02470376163623,1.11069974665188,5.76997069384733));
#17417=CARTESIAN_POINT('Ctrl Pts',(-2.03150206860296,-1.09820982237999,
5.88108263414585));
#17418=CARTESIAN_POINT('Ctrl Pts',(-0.179645428808579,-2.30235098638037,
5.99219457444435));
#17419=CARTESIAN_POINT('Ctrl Pts',(1.83658550522895,-1.40001438181273,6.10330651474285));
#17420=CARTESIAN_POINT('Ctrl Pts',(2.17246271157681,0.783202663677277,6.21441845504137));
#17421=CARTESIAN_POINT('Ctrl Pts',(0.520757933621259,2.24989134978725,6.32553039533987));
#17422=CARTESIAN_POINT('Ctrl Pts',(-1.60748926038381,1.65803443249082,6.43664233563838));
#17423=CARTESIAN_POINT('Ctrl Pts',(-2.26483986170582,-0.450648314453544,
6.54775427593688));
#17424=CARTESIAN_POINT('Ctrl Pts',(-0.850371985170964,-2.14729633892256,
6.6588662162354));
#17425=CARTESIAN_POINT('Ctrl Pts',(1.34274482878903,-1.87882089420371,6.7699781565339));
#17426=CARTESIAN_POINT('Ctrl Pts',(2.30616083080651,0.107634649639171,6.88109009683241));
#17427=CARTESIAN_POINT('Ctrl Pts',(1.16193045799902,1.99751503787814,6.99220203713092));
#17428=CARTESIAN_POINT('Ctrl Pts',(-1.04999517826429,2.05607780322851,7.10331397742942));
#17429=CARTESIAN_POINT('Ctrl Pts',(-1.87709151778098,0.84653605896511,7.1773886042951));
#17430=CARTESIAN_POINT('Ctrl Pts',(-1.94370052943366,0.200360305148756,
7.21442591772793));
#17431=CARTESIAN_POINT('Ctrl Pts',(1.05793541951256,-1.48236995244729,-0.153382721514712));
#17432=CARTESIAN_POINT('Ctrl Pts',(1.55074360006928,-1.13066339742992,-0.116345408081876));
#17433=CARTESIAN_POINT('Ctrl Pts',(2.14954808422461,0.0967392444982914,
-0.0422707812162042));
#17434=CARTESIAN_POINT('Ctrl Pts',(1.08289805597856,1.8617492085907,0.0688411590823027));
#17435=CARTESIAN_POINT('Ctrl Pts',(-0.975426428816855,1.91793473829667,
0.179953099380811));
#17436=CARTESIAN_POINT('Ctrl Pts',(-2.14083559528361,0.222108233089066,
0.291065039679317));
#17437=CARTESIAN_POINT('Ctrl Pts',(-1.34780266824982,-1.6783555537827,0.402176979977826));
#17438=CARTESIAN_POINT('Ctrl Pts',(0.678493704334455,-2.04251144516605,
0.513288920276332));
#17439=CARTESIAN_POINT('Ctrl Pts',(2.08395341218121,-0.538324680837788,
0.624400860574841));
#17440=CARTESIAN_POINT('Ctrl Pts',(1.58279885012795,1.4585917731467,0.735512800873347));
#17441=CARTESIAN_POINT('Ctrl Pts',(-0.366509073634787,2.12090550597771,
0.846624741171857));
#17442=CARTESIAN_POINT('Ctrl Pts',(-1.9804805111294,0.842817100910752,0.957736681470361));
#17443=CARTESIAN_POINT('Ctrl Pts',(-1.78247602221336,-1.20641125891655,
1.06884862176887));
#17444=CARTESIAN_POINT('Ctrl Pts',(0.0463541464078725,-2.15185423966612,
1.17996056206738));
#17445=CARTESIAN_POINT('Ctrl Pts',(1.83277253201941,-1.12853098869745,1.29107250236589));
#17446=CARTESIAN_POINT('Ctrl Pts',(1.94235147600127,0.927312111837943,1.40218444266439));
#17447=CARTESIAN_POINT('Ctrl Pts',(0.274833853990247,2.13473657748725,1.5132963829629));
#17448=CARTESIAN_POINT('Ctrl Pts',(-1.6441345417364,1.38904908974441,1.62440832326141));
#17449=CARTESIAN_POINT('Ctrl Pts',(-2.05885151110621,-0.627507781172011,
1.73552026355991));
#17450=CARTESIAN_POINT('Ctrl Pts',(-0.589884046505544,-2.06994492084524,
1.84663220385842));
#17451=CARTESIAN_POINT('Ctrl Pts',(1.4187800857734,-1.6185482736686,1.95774414415693));
#17452=CARTESIAN_POINT('Ctrl Pts',(2.12937399117781,0.313690612134129,2.06885608445544));
#17453=CARTESIAN_POINT('Ctrl Pts',(0.891761086185737,1.95892764316774,2.17996802475395));
#17454=CARTESIAN_POINT('Ctrl Pts',(-1.16174184647048,1.81190266569614,2.29107996505245));
#17455=CARTESIAN_POINT('Ctrl Pts',(-2.15234395851487,0.00713173081318942,
2.40219190535096));
#17456=CARTESIAN_POINT('Ctrl Pts',(-1.17372358532974,-1.80416416021932,
2.51330384564946));
#17457=CARTESIAN_POINT('Ctrl Pts',(0.878759942370547,-1.96479422370721,
2.62441578594798));
#17458=CARTESIAN_POINT('Ctrl Pts',(2.1272484445495,-0.327794800258781,2.73552772624649));
#17459=CARTESIAN_POINT('Ctrl Pts',(1.42947484958074,1.60911063316174,2.84663966654499));
#17460=CARTESIAN_POINT('Ctrl Pts',(-0.576153841133258,2.07380860436568,
2.9577516068435));
#17461=CARTESIAN_POINT('Ctrl Pts',(-2.0546478730846,0.641137655651238,3.068863547142));
#17462=CARTESIAN_POINT('Ctrl Pts',(-1.65330352117917,-1.37812294178502,
3.17997548744051));
#17463=CARTESIAN_POINT('Ctrl Pts',(0.260681249517398,-2.1365113297345,3.29108742773902));
#17464=CARTESIAN_POINT('Ctrl Pts',(1.93616353752793,-0.940162821976462,
3.40219936803753));
#17465=CARTESIAN_POINT('Ctrl Pts',(1.84021112721267,1.11635943278533,3.51331130833604));
#17466=CARTESIAN_POINT('Ctrl Pts',(0.0606127955645832,2.15150214150485,
3.62442324863454));
#17467=CARTESIAN_POINT('Ctrl Pts',(-1.77444139357172,1.21819256140342,3.73553518893305));
#17468=CARTESIAN_POINT('Ctrl Pts',(-1.98602370455295,-0.829665728403687,
3.84664712923155));
#17469=CARTESIAN_POINT('Ctrl Pts',(-0.380553254334539,-2.11844626942319,
3.95775906953007));
#17470=CARTESIAN_POINT('Ctrl Pts',(1.57309297035165,-1.46901799937757,4.06887100982856));
#17471=CARTESIAN_POINT('Ctrl Pts',(2.08748501162692,0.524444184281487,4.17998295012709));
#17472=CARTESIAN_POINT('Ctrl Pts',(0.691995314832617,2.038081906987,4.29109489042558));
#17473=CARTESIAN_POINT('Ctrl Pts',(-1.33661471876519,1.68703777951035,4.4022068307241));
#17474=CARTESIAN_POINT('Ctrl Pts',(-2.14232924600648,-0.207510914251802,
4.5133187710226));
#17475=CARTESIAN_POINT('Ctrl Pts',(-0.987983948286119,-1.91220372599474,
4.62443071132112));
#17476=CARTESIAN_POINT('Ctrl Pts',(1.07028759741094,-1.86738315194504,4.73554265161961));
#17477=CARTESIAN_POINT('Ctrl Pts',(2.14933164494543,-0.114056423903322,
4.84665459191812));
#17478=CARTESIAN_POINT('Ctrl Pts',(1.26190922413262,1.74362279637852,4.95776653221663));
#17479=CARTESIAN_POINT('Ctrl Pts',(-0.780059135009386,2.00602670479084,
5.06887847251514));
#17480=CARTESIAN_POINT('Ctrl Pts',(-2.10833584561709,0.433076676893185,
5.17999041281365));
#17481=CARTESIAN_POINT('Ctrl Pts',(-1.50765390340601,-1.53610379571154,
5.29110235311216));
#17482=CARTESIAN_POINT('Ctrl Pts',(0.472410578590484,-2.0998723307505,5.40221429341067));
#17483=CARTESIAN_POINT('Ctrl Pts',(2.02025744064608,-0.742425510448462,
5.51332623370916));
#17484=CARTESIAN_POINT('Ctrl Pts',(1.71972992571626,1.29428083705086,5.62443817400769));
#17485=CARTESIAN_POINT('Ctrl Pts',(-0.154211925170411,2.14682455995381,
5.73555011430617));
#17486=CARTESIAN_POINT('Ctrl Pts',(-1.88706397163077,1.03519414292605,5.8466620546047));
#17487=CARTESIAN_POINT('Ctrl Pts',(-1.89340012825184,-1.02355328634819,
5.95777399490319));
#17488=CARTESIAN_POINT('Ctrl Pts',(-0.167433094557426,-2.14583667930556,
6.0688859352017));
#17489=CARTESIAN_POINT('Ctrl Pts',(1.71173403408707,-1.3048411079894,6.17999787550022));
#17490=CARTESIAN_POINT('Ctrl Pts',(2.02477823689865,0.729960380928156,6.29110981579872));
#17491=CARTESIAN_POINT('Ctrl Pts',(0.485356699136765,2.09694325990492,6.40222175609723));
#17492=CARTESIAN_POINT('Ctrl Pts',(-1.49821180042767,1.54532090104292,6.51333369639574));
#17493=CARTESIAN_POINT('Ctrl Pts',(-2.11087556882117,-0.420013146710507,
6.62444563669424));
#17494=CARTESIAN_POINT('Ctrl Pts',(-0.792563517738235,-2.00132267958093,
6.73555757699275));
#17495=CARTESIAN_POINT('Ctrl Pts',(1.2514647512946,-1.75109825238519,6.84666951729126));
#17496=CARTESIAN_POINT('Ctrl Pts',(2.1493875297017,0.100317623388547,6.95778145758976));
#17497=CARTESIAN_POINT('Ctrl Pts',(1.08294217967889,1.86172354306503,7.06889339788828));
#17498=CARTESIAN_POINT('Ctrl Pts',(-0.978616283938414,1.91630519923899,
7.18000533818678));
#17499=CARTESIAN_POINT('Ctrl Pts',(-1.74948643933749,0.788988358607273,
7.25407996505245));
#17500=CARTESIAN_POINT('Ctrl Pts',(-1.8115673562881,0.186739769222141,7.29111727848529));
#17501=CARTESIAN_POINT('Ctrl Pts',(0.980771099081382,-1.37424797458506,
-0.0766913607573567));
#17502=CARTESIAN_POINT('Ctrl Pts',(1.43763454458697,-1.04819440065571,-0.0396540473245209));
#17503=CARTESIAN_POINT('Ctrl Pts',(1.99276307249889,0.0896832201672716,
0.034420579541151));
#17504=CARTESIAN_POINT('Ctrl Pts',(1.00391299597902,1.72595584177028,0.145532519839658));
#17505=CARTESIAN_POINT('Ctrl Pts',(-0.904280198033752,1.77804327802189,
0.256644460138166));
#17506=CARTESIAN_POINT('Ctrl Pts',(-1.98468606023822,0.205907971189911,
0.367756400436673));
#17507=CARTESIAN_POINT('Ctrl Pts',(-1.24949583869046,-1.55593866201325,
0.478868340735181));
#17508=CARTESIAN_POINT('Ctrl Pts',(0.629005328535562,-1.89353353523676,
0.589980281033688));
#17509=CARTESIAN_POINT('Ctrl Pts',(1.93195278350834,-0.499060036321655,
0.701092221332196));
#17510=CARTESIAN_POINT('Ctrl Pts',(1.46735172982485,1.35220414221434,0.812204161630702));
#17511=CARTESIAN_POINT('Ctrl Pts',(-0.339776417673698,1.96620964359423,
0.923316101929211));
#17512=CARTESIAN_POINT('Ctrl Pts',(-1.8360270502188,0.781343207854476,1.03442804222772));
#17513=CARTESIAN_POINT('Ctrl Pts',(-1.65246473002849,-1.11841731974236,
1.14553998252623));
#17514=CARTESIAN_POINT('Ctrl Pts',(0.0429731402134002,-1.99490102020845,
1.25665192282473));
#17515=CARTESIAN_POINT('Ctrl Pts',(1.69909268320277,-1.04621752681478,1.36776386312324));
#17516=CARTESIAN_POINT('Ctrl Pts',(1.80067909324543,0.859675271613291,1.47887580342175));
#17517=CARTESIAN_POINT('Ctrl Pts',(0.254787859515066,1.97903189621542,1.58998774372026));
#17518=CARTESIAN_POINT('Ctrl Pts',(-1.52421368241876,1.2877338042565,1.70109968401876));
#17519=CARTESIAN_POINT('Ctrl Pts',(-1.90868177976625,-0.581738246844747,
1.81221162431727));
#17520=CARTESIAN_POINT('Ctrl Pts',(-0.54685873442858,-1.91896605181315,
1.92332356461578));
#17521=CARTESIAN_POINT('Ctrl Pts',(1.3152962632822,-1.50049364073057,2.03443550491428));
#17522=CARTESIAN_POINT('Ctrl Pts',(1.97406044940342,0.290810460411716,2.14554744521279));
#17523=CARTESIAN_POINT('Ctrl Pts',(0.826717287733271,1.81604621811011,2.2566593855113));
#17524=CARTESIAN_POINT('Ctrl Pts',(-1.0770060313669,1.6797450355543,2.36777132580981));
#17525=CARTESIAN_POINT('Ctrl Pts',(-1.99535501965367,0.00661155240574004,
2.47888326610832));
#17526=CARTESIAN_POINT('Ctrl Pts',(-1.08811383905831,-1.67257096577485,
2.58999520640682));
#17527=CARTESIAN_POINT('Ctrl Pts',(0.814664429048569,-1.82148489852237,
2.70110714670533));
#17528=CARTESIAN_POINT('Ctrl Pts',(1.97208993715443,-0.303885908906504,
2.81221908700384));
#17529=CARTESIAN_POINT('Ctrl Pts',(1.32521096607054,1.49174436843859,2.92333102730234));
#17530=CARTESIAN_POINT('Ctrl Pts',(-0.534129990910586,1.92254792369583,
3.03444296760085));
#17531=CARTESIAN_POINT('Ctrl Pts',(-1.90478474918523,0.594373977463801,
3.14555490789936));
#17532=CARTESIAN_POINT('Ctrl Pts',(-1.53271388940651,-1.27760459415048,
3.25666684819786));
#17533=CARTESIAN_POINT('Ctrl Pts',(0.241667526092368,-1.98067720053176,
3.36777878849638));
#17534=CARTESIAN_POINT('Ctrl Pts',(1.79494249429468,-0.871588669041957,
3.47889072879488));
#17535=CARTESIAN_POINT('Ctrl Pts',(1.70598871773261,1.03493374705916,3.59000266909339));
#17536=CARTESIAN_POINT('Ctrl Pts',(0.0561917835699789,1.99457460359148,
3.70111460939189));
#17537=CARTESIAN_POINT('Ctrl Pts',(-1.64501613589106,1.12933931060827,3.81222654969041));
#17538=CARTESIAN_POINT('Ctrl Pts',(-1.8411659309162,-0.769151077947235,
3.92333848998891));
#17539=CARTESIAN_POINT('Ctrl Pts',(-0.352796235600697,-1.96392978029257,
4.03445043028742));
#17540=CARTESIAN_POINT('Ctrl Pts',(1.45835378325819,-1.36186989417907,4.14556237058593));
#17541=CARTESIAN_POINT('Ctrl Pts',(1.93522679306129,0.486191963647073,4.25667431088443));
#17542=CARTESIAN_POINT('Ctrl Pts',(0.641522150567798,1.88942708133782,4.36778625118295));
#17543=CARTESIAN_POINT('Ctrl Pts',(-1.23912392249396,1.56398761841675,4.47889819148144));
#17544=CARTESIAN_POINT('Ctrl Pts',(-1.9860707661797,-0.192375360242598,
4.59001013177996));
#17545=CARTESIAN_POINT('Ctrl Pts',(-0.915921789707908,-1.77273027769074,
4.70112207207846));
#17546=CARTESIAN_POINT('Ctrl Pts',(0.992222326509824,-1.73117885322625,
4.81223401237697));
#17547=CARTESIAN_POINT('Ctrl Pts',(1.99256241999608,-0.105737308880805,
4.92334595267548));
#17548=CARTESIAN_POINT('Ctrl Pts',(1.1698673414902,1.61644540379926,5.03445789297399));
#17549=CARTESIAN_POINT('Ctrl Pts',(-0.723162719652709,1.85970994047142,
5.1455698332725));
#17550=CARTESIAN_POINT('Ctrl Pts',(-1.95455679656824,0.401488673645819,
5.25668177357099));
#17551=CARTESIAN_POINT('Ctrl Pts',(-1.39768774974859,-1.42406254695323,
5.36779371386952));
#17552=CARTESIAN_POINT('Ctrl Pts',(0.437953615916691,-1.94671059856343,
5.47890565416801));
#17553=CARTESIAN_POINT('Ctrl Pts',(1.87290270648346,-0.688274038697066,
5.59001759446653));
#17554=CARTESIAN_POINT('Ctrl Pts',(1.59429524549334,1.19987781452597,5.70112953476503));
#17555=CARTESIAN_POINT('Ctrl Pts',(-0.142963924405265,1.99023819825497,
5.81224147506354));
#17556=CARTESIAN_POINT('Ctrl Pts',(-1.74942418162531,0.959688539200224,
5.92335341536204));
#17557=CARTESIAN_POINT('Ctrl Pts',(-1.75529818790071,-0.948896750316397,
6.03446535566056));
#17558=CARTESIAN_POINT('Ctrl Pts',(-0.155220760306272,-1.98932237223074,
6.14557729595905));
#17559=CARTESIAN_POINT('Ctrl Pts',(1.58688256294519,-1.20966783416606,6.25668923625758));
#17560=CARTESIAN_POINT('Ctrl Pts',(1.8770937622205,0.676718098179033,6.36780117655607));
#17561=CARTESIAN_POINT('Ctrl Pts',(0.449955464652266,1.94399517002259,6.47891311685458));
#17562=CARTESIAN_POINT('Ctrl Pts',(-1.38893434047152,1.43260736959501,6.59002505715309));
#17563=CARTESIAN_POINT('Ctrl Pts',(-1.95691127593653,-0.389377978967469,
6.7011369974516));
#17564=CARTESIAN_POINT('Ctrl Pts',(-0.734755050305503,-1.8553490202393,
6.8122489377501));
#17565=CARTESIAN_POINT('Ctrl Pts',(1.16018467380016,-1.62337561056666,6.92336087804862));
#17566=CARTESIAN_POINT('Ctrl Pts',(1.99261422859689,0.0930005971379224,
7.03447281834711));
#17567=CARTESIAN_POINT('Ctrl Pts',(1.00395390135875,1.72593204825193,7.14558475864564));
#17568=CARTESIAN_POINT('Ctrl Pts',(-0.907237389612538,1.77653259524947,
7.25669669894413));
#17569=CARTESIAN_POINT('Ctrl Pts',(-1.62188136089401,0.731440658249439,
7.33077132580981));
#17570=CARTESIAN_POINT('Ctrl Pts',(-1.67943418314253,0.173119233295526,
7.36780863924264));
#17571=CARTESIAN_POINT('Ctrl Pts',(0.903606778650207,-1.26612599672284,
-1.38777878078145E-15));
#17572=CARTESIAN_POINT('Ctrl Pts',(1.32452548910467,-0.965725403881512,
0.0370373134328344));
#17573=CARTESIAN_POINT('Ctrl Pts',(1.83597806077316,0.082627195836251,0.111111940298506));
#17574=CARTESIAN_POINT('Ctrl Pts',(0.924927935979477,1.59016247494986,0.222223880597014));
#17575=CARTESIAN_POINT('Ctrl Pts',(-0.833133967250649,1.63815181774712,
0.333335820895521));
#17576=CARTESIAN_POINT('Ctrl Pts',(-1.82853652519283,0.189707709290757,
0.444447761194028));
#17577=CARTESIAN_POINT('Ctrl Pts',(-1.15118900913109,-1.43352177024381,
0.555559701492536));
#17578=CARTESIAN_POINT('Ctrl Pts',(0.579516952736672,-1.74455562530747,
0.666671641791043));
#17579=CARTESIAN_POINT('Ctrl Pts',(1.77995215483547,-0.45979539180552,0.777783582089551));
#17580=CARTESIAN_POINT('Ctrl Pts',(1.35190460952174,1.24581651128198,0.888895522388059));
#17581=CARTESIAN_POINT('Ctrl Pts',(-0.313043761712607,1.81151378121076,
1.00000746268657));
#17582=CARTESIAN_POINT('Ctrl Pts',(-1.6915735893082,0.719869314798195,1.11111940298507));
#17583=CARTESIAN_POINT('Ctrl Pts',(-1.52245343784362,-1.03042338056816,
1.22223134328358));
#17584=CARTESIAN_POINT('Ctrl Pts',(0.0395921340189295,-1.83794780075079,
1.33334328358209));
#17585=CARTESIAN_POINT('Ctrl Pts',(1.56541283438613,-0.96390406493211,1.44445522388059));
#17586=CARTESIAN_POINT('Ctrl Pts',(1.65900671048959,0.792038431388639,1.55556716417911));
#17587=CARTESIAN_POINT('Ctrl Pts',(0.234741865039883,1.82332721494359,1.66667910447761));
#17588=CARTESIAN_POINT('Ctrl Pts',(-1.40429282310112,1.18641851876859,1.77779104477612));
#17589=CARTESIAN_POINT('Ctrl Pts',(-1.7585120484263,-0.535968712517482,
1.88890298507462));
#17590=CARTESIAN_POINT('Ctrl Pts',(-0.503833422351614,-1.76798718278107,
2.00001492537314));
#17591=CARTESIAN_POINT('Ctrl Pts',(1.211812440791,-1.38243900779253,2.11112686567164));
#17592=CARTESIAN_POINT('Ctrl Pts',(1.81874690762903,0.2679303086893,2.22223880597015));
#17593=CARTESIAN_POINT('Ctrl Pts',(0.761673489280804,1.67316479305249,2.33335074626865));
#17594=CARTESIAN_POINT('Ctrl Pts',(-0.99227021626331,1.54758740541246,2.44446268656716));
#17595=CARTESIAN_POINT('Ctrl Pts',(-1.83836608079246,0.00609137399829168,
2.55557462686567));
#17596=CARTESIAN_POINT('Ctrl Pts',(-1.00250409278689,-1.54097777133038,
2.66668656716418));
#17597=CARTESIAN_POINT('Ctrl Pts',(0.750568915726592,-1.67817557333754,
2.77779850746269));
#17598=CARTESIAN_POINT('Ctrl Pts',(1.81693142975936,-0.279977017554228,
2.8889104477612));
#17599=CARTESIAN_POINT('Ctrl Pts',(1.22094708256035,1.37437810371544,3.0000223880597));
#17600=CARTESIAN_POINT('Ctrl Pts',(-0.492106140687917,1.77128724302598,
3.11113432835821));
#17601=CARTESIAN_POINT('Ctrl Pts',(-1.75492162528586,0.547610299276366,
3.22224626865671));
#17602=CARTESIAN_POINT('Ctrl Pts',(-1.41212425763385,-1.17708624651594,
3.33335820895523));
#17603=CARTESIAN_POINT('Ctrl Pts',(0.222653802667342,-1.82484307132901,
3.44447014925373));
#17604=CARTESIAN_POINT('Ctrl Pts',(1.65372145106143,-0.803014516107455,
3.55558208955224));
#17605=CARTESIAN_POINT('Ctrl Pts',(1.57176630825256,0.953508061332994,3.66669402985075));
#17606=CARTESIAN_POINT('Ctrl Pts',(0.0517707715753711,1.83764706567811,
3.77780597014925));
#17607=CARTESIAN_POINT('Ctrl Pts',(-1.5155908782104,1.04048605981312,3.88891791044777));
#17608=CARTESIAN_POINT('Ctrl Pts',(-1.69630815727945,-0.708636427490783,
4.00002985074626));
#17609=CARTESIAN_POINT('Ctrl Pts',(-0.325039216866852,-1.80941329116195,
4.11114179104478));
#17610=CARTESIAN_POINT('Ctrl Pts',(1.34361459616473,-1.25472178898058,4.22225373134328));
#17611=CARTESIAN_POINT('Ctrl Pts',(1.78296857449566,0.447939743012656,4.3333656716418));
#17612=CARTESIAN_POINT('Ctrl Pts',(0.591048986302979,1.74077225568864,4.44447761194029));
#17613=CARTESIAN_POINT('Ctrl Pts',(-1.14163312622272,1.44093745732314,4.55558955223881));
#17614=CARTESIAN_POINT('Ctrl Pts',(-1.82981228635293,-0.177239806233389,
4.66670149253731));
#17615=CARTESIAN_POINT('Ctrl Pts',(-0.843859631129698,-1.63325682938675,
4.77781343283583));
#17616=CARTESIAN_POINT('Ctrl Pts',(0.914157055608714,-1.59497455450745,
4.88892537313433));
#17617=CARTESIAN_POINT('Ctrl Pts',(1.83579319504673,-0.0974181938582904,
5.00003731343284));
#17618=CARTESIAN_POINT('Ctrl Pts',(1.07782545884778,1.48926801121999,5.11114925373134));
#17619=CARTESIAN_POINT('Ctrl Pts',(-0.666266304296033,1.713393176152,5.22226119402985));
#17620=CARTESIAN_POINT('Ctrl Pts',(-1.80077774751939,0.369900670398456,
5.33337313432836));
#17621=CARTESIAN_POINT('Ctrl Pts',(-1.28772159609117,-1.31202129819493,
5.44448507462686));
#17622=CARTESIAN_POINT('Ctrl Pts',(0.403496653242899,-1.79354886637635,
5.55559701492538));
#17623=CARTESIAN_POINT('Ctrl Pts',(1.72554797232085,-0.634122566945669,
5.66670895522387));
#17624=CARTESIAN_POINT('Ctrl Pts',(1.46886056527041,1.10547479200108,5.77782089552239));
#17625=CARTESIAN_POINT('Ctrl Pts',(-0.131715923640121,1.83365183655613,
5.88893283582089));
#17626=CARTESIAN_POINT('Ctrl Pts',(-1.61178439161985,0.884182935474394,
6.0000447761194));
#17627=CARTESIAN_POINT('Ctrl Pts',(-1.61719624754958,-0.874240214284601,
6.11115671641792));
#17628=CARTESIAN_POINT('Ctrl Pts',(-0.143008426055117,-1.83280806515592,
6.2222686567164));
#17629=CARTESIAN_POINT('Ctrl Pts',(1.4620310918033,-1.11449456034272,6.33338059701493));
#17630=CARTESIAN_POINT('Ctrl Pts',(1.72940928754233,0.623475815429911,6.44449253731343));
#17631=CARTESIAN_POINT('Ctrl Pts',(0.414554230167772,1.79104708014026,6.55560447761194));
#17632=CARTESIAN_POINT('Ctrl Pts',(-1.27965688051538,1.3198938381471,6.66671641791045));
#17633=CARTESIAN_POINT('Ctrl Pts',(-1.80294698305189,-0.358742811224428,
6.77782835820896));
#17634=CARTESIAN_POINT('Ctrl Pts',(-0.676946582872774,-1.70937536089767,
6.88894029850746));
#17635=CARTESIAN_POINT('Ctrl Pts',(1.06890459630572,-1.49565296874813,7.00005223880597));
#17636=CARTESIAN_POINT('Ctrl Pts',(1.83584092749207,0.0856835708872964,
7.11116417910447));
#17637=CARTESIAN_POINT('Ctrl Pts',(0.924965623038614,1.59014055343882,7.22227611940298));
#17638=CARTESIAN_POINT('Ctrl Pts',(-0.835858495286665,1.63675999125994,
7.33338805970149));
#17639=CARTESIAN_POINT('Ctrl Pts',(-1.49427628245053,0.673892957891604,
7.40746268656716));
#17640=CARTESIAN_POINT('Ctrl Pts',(-1.54730100999696,0.159498697368912,
7.4445));
#17641=CARTESIAN_POINT('',(0.903606778650208,-1.26612599672284,0.));
#17642=CARTESIAN_POINT('Ctrl Pts',(0.903606778650207,-1.26612599672284,
-1.38777878078145E-15));
#17643=CARTESIAN_POINT('Ctrl Pts',(1.32452548910467,-0.965725403881512,
0.0370373134328344));
#17644=CARTESIAN_POINT('Ctrl Pts',(1.83597806077316,0.082627195836251,0.111111940298506));
#17645=CARTESIAN_POINT('Ctrl Pts',(0.924927935979477,1.59016247494986,0.222223880597014));
#17646=CARTESIAN_POINT('Ctrl Pts',(-0.833133967250649,1.63815181774712,
0.333335820895521));
#17647=CARTESIAN_POINT('Ctrl Pts',(-1.5310648992002,0.622568787117098,0.411242452161949));
#17648=CARTESIAN_POINT('Ctrl Pts',(-1.55772948793458,0.0543297678623362,
0.452111769995541));
#17649=CARTESIAN_POINT('Ctrl Pts',(-1.55735958542387,0.00101297198046621,
0.455943774396298));
#17650=CARTESIAN_POINT('Ctrl Pts',(0.863568564283469,1.75641400930303,0.));
#17651=CARTESIAN_POINT('Ctrl Pts',(0.902603531943078,1.7324423702308,2.28859211685802E-17));
#17652=CARTESIAN_POINT('Ctrl Pts',(0.940676776691071,1.70703651305647,-1.38032481715684E-16));
#17653=CARTESIAN_POINT('Ctrl Pts',(0.977697814042708,1.68019172043607,-1.28369537222284E-16));
#17654=CARTESIAN_POINT('Ctrl Pts',(1.03585714935899,1.63801906923031,-1.20927094907836E-16));
#17655=CARTESIAN_POINT('Ctrl Pts',(1.09142188330105,1.59229630788867,-2.7046412047637E-16));
#17656=CARTESIAN_POINT('Ctrl Pts',(1.14423064795477,1.54336420856895,-1.97758476261356E-16));
#17657=CARTESIAN_POINT('Ctrl Pts',(1.16946834979149,1.51997919396061,-1.63011907532148E-16));
#17658=CARTESIAN_POINT('Ctrl Pts',(1.19407597424497,1.49586072902399,-7.62289135782024E-17));
#17659=CARTESIAN_POINT('Ctrl Pts',(1.21803226410959,1.47104407323701,-6.59194920871187E-17));
#17660=CARTESIAN_POINT('Ctrl Pts',(1.23017793652576,1.45846220127952,-6.0692687062697E-17));
#17661=CARTESIAN_POINT('Ctrl Pts',(1.24215614940632,1.44570084965787,-2.95883426371776E-16));
#17662=CARTESIAN_POINT('Ctrl Pts',(1.25396388375076,1.43276453675822,-3.36536354339501E-16));
#17663=CARTESIAN_POINT('Ctrl Pts',(1.2638543668245,1.42192872524363,-3.70588365016071E-16));
#17664=CARTESIAN_POINT('Ctrl Pts',(1.2736185550329,1.41097745381189,1.09305947039191E-16));
#17665=CARTESIAN_POINT('Ctrl Pts',(1.28325381741352,1.39991535359824,9.71445146547012E-17));
#17666=CARTESIAN_POINT('Ctrl Pts',(1.33014189367208,1.34608385655041,3.79633375853411E-17));
#17667=CARTESIAN_POINT('Ctrl Pts',(1.37399192615748,1.28961736627304,-2.11573378166283E-16));
#17668=CARTESIAN_POINT('Ctrl Pts',(1.4146405205773,1.23085017638072,-2.98372437868011E-16));
#17669=CARTESIAN_POINT('Ctrl Pts',(1.44368223570237,1.18886348503472,-3.60386723994296E-16));
#17670=CARTESIAN_POINT('Ctrl Pts',(1.47108885988106,1.14570172941536,-3.55315850605615E-16));
#17671=CARTESIAN_POINT('Ctrl Pts',(1.49678522627473,1.10148200990233,-3.88578058618805E-16));
#17672=CARTESIAN_POINT('Ctrl Pts',(1.51163132719121,1.07593402353214,-4.0779533196023E-16));
#17673=CARTESIAN_POINT('Ctrl Pts',(1.52590630204136,1.05003284136309,-4.46468072791598E-16));
#17674=CARTESIAN_POINT('Ctrl Pts',(1.53959352057452,1.02380089191946,-4.5102810375397E-16));
#17675=CARTESIAN_POINT('Ctrl Pts',(1.54536419749809,1.0127412230066,-4.5295066131244E-16));
#17676=CARTESIAN_POINT('Ctrl Pts',(1.55102598614157,1.00163115224642,-3.28801907372083E-16));
#17677=CARTESIAN_POINT('Ctrl Pts',(1.55657733146951,0.990474109820403,-3.19189119579733E-16));
#17678=CARTESIAN_POINT('Ctrl Pts',(1.58759135376405,0.928142415050821,-2.65484801564386E-16));
#17679=CARTESIAN_POINT('Ctrl Pts',(1.61517084797965,0.864329379202861,-6.67259587666608E-16));
#17680=CARTESIAN_POINT('Ctrl Pts',(1.6391617363075,0.799343273084874,-5.82867087928207E-16));
#17681=CARTESIAN_POINT('Ctrl Pts',(1.66256147081466,0.735958474279834,-5.00554083870677E-16));
#17682=CARTESIAN_POINT('Ctrl Pts',(1.68254736306605,0.671456731546573,9.30631015772363E-17));
#17683=CARTESIAN_POINT('Ctrl Pts',(1.69892809919455,0.606119085630755,1.11022302462516E-16));
#17684=CARTESIAN_POINT('Ctrl Pts',(1.70969727271493,0.563164212250211,1.2282920473501E-16));
#17685=CARTESIAN_POINT('Ctrl Pts',(1.71890726464806,0.519847981128071,-1.31890518419189E-16));
#17686=CARTESIAN_POINT('Ctrl Pts',(1.72649157325935,0.476251973430995,-1.38777878078145E-16));
#17687=CARTESIAN_POINT('Ctrl Pts',(1.73286785345701,0.439599936333954,-1.44568219328534E-16));
#17688=CARTESIAN_POINT('Ctrl Pts',(1.73809492661148,0.402750145627894,-3.72078883249312E-16));
#17689=CARTESIAN_POINT('Ctrl Pts',(1.74212769993621,0.365752815321986,-4.16333634234434E-16));
#17690=CARTESIAN_POINT('Ctrl Pts',(1.74338298809393,0.354236593888137,-4.30108885249319E-16));
#17691=CARTESIAN_POINT('Ctrl Pts',(1.7445224615788,0.34270569873049,-4.2222380310258E-18));
#17692=CARTESIAN_POINT('Ctrl Pts',(1.74554359854572,0.331176868161872,-1.38777878078145E-17));
#17693=CARTESIAN_POINT('Ctrl Pts',(1.75129265664821,0.266268908759598,-6.82390718242887E-17));
#17694=CARTESIAN_POINT('Ctrl Pts',(1.75330855751176,0.201308359017101,-1.61972025925174E-16));
#17695=CARTESIAN_POINT('Ctrl Pts',(1.75142416657778,0.13655560768634,-1.38777878078145E-16));
#17696=CARTESIAN_POINT('Ctrl Pts',(1.75088156113035,0.117910222074166,-1.32099183788468E-16));
#17697=CARTESIAN_POINT('Ctrl Pts',(1.75001524326664,0.0992821075343112,
-1.58618989379829E-17));
#17698=CARTESIAN_POINT('Ctrl Pts',(1.74882042289714,0.0806776277944099,
0.));
#17699=CARTESIAN_POINT('Ctrl Pts',(1.74441970791246,0.0121543460832101,
6.07280452025807E-17));
#17700=CARTESIAN_POINT('Ctrl Pts',(1.735566761163,-0.0560504444942819,-6.11382253507945E-17));
#17701=CARTESIAN_POINT('Ctrl Pts',(1.72245455146386,-0.123599567095003,
-1.38777878078145E-16));
#17702=CARTESIAN_POINT('Ctrl Pts',(1.7106535204694,-0.184393995170097,-2.08653815792513E-16));
#17703=CARTESIAN_POINT('Ctrl Pts',(1.69540126258663,-0.244657625690558,
-3.30909447568271E-16));
#17704=CARTESIAN_POINT('Ctrl Pts',(1.67680583516799,-0.304119468797943,
-3.05311331771918E-16));
#17705=CARTESIAN_POINT('Ctrl Pts',(1.673496966793,-0.314700102829495,-3.00756405772578E-16));
#17706=CARTESIAN_POINT('Ctrl Pts',(1.67008375904048,-0.325250056291554,
1.12130257435328E-16));
#17707=CARTESIAN_POINT('Ctrl Pts',(1.66656954022458,-0.335760782955591,
1.11022302462516E-16));
#17708=CARTESIAN_POINT('Ctrl Pts',(1.64601748634937,-0.397230211008769,
1.04542697325368E-16));
#17709=CARTESIAN_POINT('Ctrl Pts',(1.62199078115275,-0.457436083404927,
4.89063387979405E-18));
#17710=CARTESIAN_POINT('Ctrl Pts',(1.59467603738004,-0.516104439016194,
-1.11022302462516E-16));
#17711=CARTESIAN_POINT('Ctrl Pts',(1.56746949320957,-0.574540396593861,
-2.26476082617573E-16));
#17712=CARTESIAN_POINT('Ctrl Pts',(1.53700015167997,-0.631451830043097,
-2.65447621135955E-16));
#17713=CARTESIAN_POINT('Ctrl Pts',(1.50341281573621,-0.68653552753498,-3.60822483003176E-16));
#17714=CARTESIAN_POINT('Ctrl Pts',(1.4705131167318,-0.740491490894733,-4.54244725638714E-16));
#17715=CARTESIAN_POINT('Ctrl Pts',(1.43462103920338,-0.792694411910378,
-4.2831431104574E-16));
#17716=CARTESIAN_POINT('Ctrl Pts',(1.39584581076301,-0.842817530414533,
-5.27355936696949E-16));
#17717=CARTESIAN_POINT('Ctrl Pts',(1.38890062306969,-0.851795284506205,
-5.45095682077361E-16));
#17718=CARTESIAN_POINT('Ctrl Pts',(1.38186288427344,-0.860706190744767,
2.35960662867998E-16));
#17719=CARTESIAN_POINT('Ctrl Pts',(1.37473315631241,-0.86954820289757,2.4980018054066E-16));
#17720=CARTESIAN_POINT('Ctrl Pts',(1.36794195322354,-0.877970389630667,
2.62982587454478E-16));
#17721=CARTESIAN_POINT('Ctrl Pts',(1.36107048536455,-0.886326025058287,
-6.35152333120316E-18));
#17722=CARTESIAN_POINT('Ctrl Pts',(1.35412452302825,-0.894607674989563,
0.));
#17723=CARTESIAN_POINT('Ctrl Pts',(1.31424959800426,-0.942150427756674,
3.64624085702422E-17));
#17724=CARTESIAN_POINT('Ctrl Pts',(1.2718724912058,-0.987319961554271,-3.18360401148313E-16));
#17725=CARTESIAN_POINT('Ctrl Pts',(1.22713193424969,-1.02984905091596,-2.22044604925031E-16));
#17726=CARTESIAN_POINT('Ctrl Pts',(1.18319618732353,-1.0716131109617,-1.27461373607439E-16));
#17727=CARTESIAN_POINT('Ctrl Pts',(1.13698054744349,-1.11083140282356,-2.10671899724563E-16));
#17728=CARTESIAN_POINT('Ctrl Pts',(1.08859303083371,-1.14720695088303,-2.77555756156289E-16));
#17729=CARTESIAN_POINT('Ctrl Pts',(1.04174975410163,-1.18242160919609,-3.42305080264122E-16));
#17730=CARTESIAN_POINT('Ctrl Pts',(0.992870408249348,-1.21497237243561,
-3.26158703430296E-16));
#17731=CARTESIAN_POINT('Ctrl Pts',(0.942040458977608,-1.24454244204819,
-3.60822483003176E-16));
#17732=CARTESIAN_POINT('Ctrl Pts',(0.92935042596986,-1.25192480549339,-3.69476524828035E-16));
#17733=CARTESIAN_POINT('Ctrl Pts',(0.916538776387811,-1.25912113789668,
-6.13893683198417E-17));
#17734=CARTESIAN_POINT('Ctrl Pts',(0.903606778650223,-1.26612599672282,
-5.55111512312578E-17));
#17735=CARTESIAN_POINT('Ctrl Pts',(0.0849160311154397,1.9485495525967,7.04599999999999));
#17736=CARTESIAN_POINT('Ctrl Pts',(0.400605874250757,1.93520776532856,7.0280673457103));
#17737=CARTESIAN_POINT('Ctrl Pts',(0.713151734000586,1.84952766933244,7.01013469142061));
#17738=CARTESIAN_POINT('Ctrl Pts',(0.983981247423036,1.69229543406338,6.99220203713092));
#17739=CARTESIAN_POINT('Ctrl Pts',(1.54334058226818,1.36755490846516,6.95516472369808));
#17740=CARTESIAN_POINT('Ctrl Pts',(1.92475070653735,0.737594779052165,6.91812741026524));
#17741=CARTESIAN_POINT('Ctrl Pts',(1.95488643500235,0.0915387903718514,
6.88109009683241));
#17742=CARTESIAN_POINT('Ctrl Pts',(1.98502216346735,-0.554517198308454,
6.84405278339957));
#17743=CARTESIAN_POINT('Ctrl Pts',(1.6638834961282,-1.21666904625608,6.80701546996674));
#17744=CARTESIAN_POINT('Ctrl Pts',(1.13779469346529,-1.59249087768303,6.7699781565339));
#17745=CARTESIAN_POINT('Ctrl Pts',(0.611705890802371,-1.96831270910999,
6.73294084310107));
#17746=CARTESIAN_POINT('Ctrl Pts',(-0.119333047184302,-2.05780452401628,
6.69590352966823));
#17747=CARTESIAN_POINT('Ctrl Pts',(-0.720597162266781,-1.81977576072458,
6.65886621623539));
#17748=CARTESIAN_POINT('Ctrl Pts',(-1.32186127734926,-1.58174699743288,
6.62182890280256));
#17749=CARTESIAN_POINT('Ctrl Pts',(-1.79335056952755,-1.0161976559432,6.58479158936972));
#17750=CARTESIAN_POINT('Ctrl Pts',(-1.91953678206301,-0.381975860707627,
6.54775427593688));
#17751=CARTESIAN_POINT('Ctrl Pts',(-1.94439039128642,-0.257059672615188,
6.540459414666));
#17752=CARTESIAN_POINT('Ctrl Pts',(-1.9558486040335,-0.129479463263859,
6.53316455339512));
#17753=CARTESIAN_POINT('Ctrl Pts',(-1.95467666345581,-0.00169153748172557,
6.52586969212423));
#17754=CARTESIAN_POINT('Origin',(0.,0.,-1.2940562256037));
#17755=CARTESIAN_POINT('',(-0.903606778650191,-1.26612599672285,1.38777878078145E-16));
#17756=CARTESIAN_POINT('Ctrl Pts',(-0.905552056217056,-1.26793026328003,
8.26433105977076E-16));
#17757=CARTESIAN_POINT('Ctrl Pts',(-0.513280080436939,-1.54506079646518,
0.0345343505799217));
#17758=CARTESIAN_POINT('Ctrl Pts',(0.58913651448779,-1.72157402054048,0.106143938272268));
#17759=CARTESIAN_POINT('Ctrl Pts',(1.77597071143275,-0.477272995959146,
0.214828763077039));
#17760=CARTESIAN_POINT('Ctrl Pts',(1.3630442868689,1.23477489449879,0.326054474414316));
#17761=CARTESIAN_POINT('Ctrl Pts',(-0.299513989741265,1.81437004394786,
0.437280185751592));
#17762=CARTESIAN_POINT('Ctrl Pts',(-1.41424275662139,0.944368549815884,
0.526614102814722));
#17763=CARTESIAN_POINT('Ctrl Pts',(-1.55418552513067,0.213449522874851,
0.578872782765425));
#17764=CARTESIAN_POINT('Ctrl Pts',(-1.55327638232574,0.000749985450955847,
0.594056225603703));
#17765=CARTESIAN_POINT('Origin',(0.,0.,0.));
#17766=CARTESIAN_POINT('Ctrl Pts',(-0.685825729128727,1.39614588036675,
-0.230074082272066));
#17767=CARTESIAN_POINT('Ctrl Pts',(-1.15044430012221,1.1679123019855,-0.19299884515964));
#17768=CARTESIAN_POINT('Ctrl Pts',(-1.8258407957124,0.215070471435756,-0.118848370934789));
#17769=CARTESIAN_POINT('Ctrl Pts',(-1.16856980438922,-1.42158824274557,
-0.0076226595975132));
#17770=CARTESIAN_POINT('Ctrl Pts',(0.561390129169046,-1.75066389321976,
0.103603051739764));
#17771=CARTESIAN_POINT('Ctrl Pts',(1.77597071143275,-0.477272995959146,
0.214828763077039));
#17772=CARTESIAN_POINT('Ctrl Pts',(1.3630442868689,1.23477489449879,0.326054474414316));
#17773=CARTESIAN_POINT('Ctrl Pts',(-0.299513989741265,1.81437004394786,
0.437280185751592));
#17774=CARTESIAN_POINT('Ctrl Pts',(-1.68741350339127,0.731169639996686,
0.548505897088869));
#17775=CARTESIAN_POINT('Ctrl Pts',(-1.52862817745114,-1.02241621535808,
0.659731608426144));
#17776=CARTESIAN_POINT('Ctrl Pts',(0.0313843551128396,-1.83872969125081,
0.770957319763422));
#17777=CARTESIAN_POINT('Ctrl Pts',(1.56261245507102,-0.969643437172017,
0.882183031100698));
#17778=CARTESIAN_POINT('Ctrl Pts',(1.66150197094076,0.788277540412492,0.993408742437974));
#17779=CARTESIAN_POINT('Ctrl Pts',(0.237394066880885,1.82362194812979,1.10463445377525));
#17780=CARTESIAN_POINT('Ctrl Pts',(-1.40431546877471,1.18737513564603,1.21586016511253));
#17781=CARTESIAN_POINT('Ctrl Pts',(-1.75877981175223,-0.537266275957094,
1.3270858764498));
#17782=CARTESIAN_POINT('Ctrl Pts',(-0.501082205369057,-1.76942810040879,
1.43831158778708));
#17783=CARTESIAN_POINT('Ctrl Pts',(1.21592516185098,-1.37966899434435,1.54953729912436));
#17784=CARTESIAN_POINT('Ctrl Pts',(1.8183716526183,0.274745208061178,1.66076301046163));
#17785=CARTESIAN_POINT('Ctrl Pts',(0.754032712405612,1.67731773070425,1.77198872179891));
#17786=CARTESIAN_POINT('Ctrl Pts',(-1.00147988107901,1.54240019271928,1.88321443313619));
#17787=CARTESIAN_POINT('Ctrl Pts',(-1.83899975790172,-0.00633731701985082,
1.99444014447346));
#17788=CARTESIAN_POINT('Ctrl Pts',(-0.990825815880477,-1.5492657736205,
2.10566585581074));
#17789=CARTESIAN_POINT('Ctrl Pts',(0.765574959497512,-1.6720811124538,2.21689156714802));
#17790=CARTESIAN_POINT('Ctrl Pts',(1.82022199392772,-0.262206313316451,
2.32811727848529));
#17791=CARTESIAN_POINT('Ctrl Pts',(1.20638759997596,1.38801628675575,2.43934298982257));
#17792=CARTESIAN_POINT('Ctrl Pts',(-0.513265374585843,1.76593287340023,
2.55056870115984));
#17793=CARTESIAN_POINT('Ctrl Pts',(-1.76244071170529,0.525131406868061,
2.66179441249712));
#17794=CARTESIAN_POINT('Ctrl Pts',(-1.39609903883734,-1.19702453193727,
2.77302012383439));
#17795=CARTESIAN_POINT('Ctrl Pts',(0.249957593646744,-1.82194441691009,
2.88424583517168));
#17796=CARTESIAN_POINT('Ctrl Pts',(1.6668940398915,-0.776804039943688,2.99547154650895));
#17797=CARTESIAN_POINT('Ctrl Pts',(1.55589501744036,0.980383063583733,3.10669725784622));
#17798=CARTESIAN_POINT('Ctrl Pts',(0.0187062518377651,1.83891553174339,
3.2179229691835));
#17799=CARTESIAN_POINT('Ctrl Pts',(-1.53562934193987,1.01183139943408,3.32914868052078));
#17800=CARTESIAN_POINT('Ctrl Pts',(-1.68235144492823,-0.742734052303713,
3.44037439185806));
#17801=CARTESIAN_POINT('Ctrl Pts',(-0.286969261786828,-1.81648256240041,
3.55160010319533));
#17802=CARTESIAN_POINT('Ctrl Pts',(1.37145934362907,-1.22517734450477,3.66282581453261));
#17803=CARTESIAN_POINT('Ctrl Pts',(1.77275862659963,0.489169815626649,3.77405152586988));
#17804=CARTESIAN_POINT('Ctrl Pts',(0.549083125265984,1.75512620009375,3.88527723720716));
#17805=CARTESIAN_POINT('Ctrl Pts',(-1.17790186202284,1.41227032121617,3.99650294854444));
#17806=CARTESIAN_POINT('Ctrl Pts',(-1.82517932708368,-0.225123700760077,
4.10772865988171));
#17807=CARTESIAN_POINT('Ctrl Pts',(-0.799431294618187,-1.65616118233816,
4.21895437121899));
#17808=CARTESIAN_POINT('Ctrl Pts',(0.959104426053338,-1.56910132141185,
4.33018008255627));
#17809=CARTESIAN_POINT('Ctrl Pts',(1.83849028118038,-0.0437463405035559,
4.44140579389354));
#17810=CARTESIAN_POINT('Ctrl Pts',(1.0326493363287,1.52170812080878,4.55263150523082));
#17811=CARTESIAN_POINT('Ctrl Pts',(-0.719755403894915,1.69230978744094,
4.6638572165681));
#17812=CARTESIAN_POINT('Ctrl Pts',(-1.81240626272056,0.311678989548955,
4.77508292790537));
#17813=CARTESIAN_POINT('Ctrl Pts',(-1.24373988019232,-1.35464806069341,
4.88630863924265));
#17814=CARTESIAN_POINT('Ctrl Pts',(0.464983542380115,-1.77925562259896,
4.99753435057992));
#17815=CARTESIAN_POINT('Ctrl Pts',(1.74748619395055,-0.572933012383953,
5.1087600619172));
#17816=CARTESIAN_POINT('Ctrl Pts',(1.42817970701863,1.15856074316792,5.21998577325448));
#17817=CARTESIAN_POINT('Ctrl Pts',(-0.20024807751692,1.82807576816643,5.33121148459175));
#17818=CARTESIAN_POINT('Ctrl Pts',(-1.64512115233065,0.821910272029074,
5.44243719592903));
#17819=CARTESIAN_POINT('Ctrl Pts',(-1.58201670345687,-0.937647879740503,
5.55366290726631));
#17820=CARTESIAN_POINT('Ctrl Pts',(-0.0687781849042931,-1.83772416168987,
5.66488861860358));
#17821=CARTESIAN_POINT('Ctrl Pts',(1.50750444735784,-1.05327561457109,5.77611432994086));
#17822=CARTESIAN_POINT('Ctrl Pts',(1.70195476716013,0.696642984640571,5.88734004127814));
#17823=CARTESIAN_POINT('Ctrl Pts',(0.336330007005007,1.80799440678846,5.99856575261541));
#17824=CARTESIAN_POINT('Ctrl Pts',(-1.33758382509627,1.26207070464844,6.10979146395269));
#17825=CARTESIAN_POINT('Ctrl Pts',(-1.78542595464098,-0.440709020390059,
6.22101717528996));
#17826=CARTESIAN_POINT('Ctrl Pts',(-0.59667036110871,-1.73952595846347,
6.33224288662724));
#17827=CARTESIAN_POINT('Ctrl Pts',(1.13899278941852,-1.44381691390763,6.44346859796452));
#17828=CARTESIAN_POINT('Ctrl Pts',(1.83065601360088,0.17532136832598,6.5546943093018));
#17829=CARTESIAN_POINT('Ctrl Pts',(0.844193344579619,1.63380261073593,6.66592002063907));
#17830=CARTESIAN_POINT('Ctrl Pts',(-0.915934603694247,1.5945880622222,6.77714573197635));
#17831=CARTESIAN_POINT('Ctrl Pts',(-1.83677508915277,0.093893769326276,
6.88837144331362));
#17832=CARTESIAN_POINT('Ctrl Pts',(-1.07340561084952,-1.49320523543669,
6.99959715465089));
#17833=CARTESIAN_POINT('Ctrl Pts',(0.672826183539381,-1.71093187207897,
7.11082286598819));
#17834=CARTESIAN_POINT('Ctrl Pts',(1.80435891657647,-0.361603954366771,
7.22204857732544));
#17835=CARTESIAN_POINT('Ctrl Pts',(1.27791236939833,1.32169962363241,7.33327428866273));
#17836=CARTESIAN_POINT('Ctrl Pts',(0.152038852759137,1.63230677878407,7.40742476288758));
#17837=CARTESIAN_POINT('Ctrl Pts',(-0.352169241380528,1.51510959188617,
7.44450000000001));
#17838=CARTESIAN_POINT('Ctrl Pts',(-0.744392439309327,1.51537102412035,
-0.153382721514711));
#17839=CARTESIAN_POINT('Ctrl Pts',(-1.24868753458029,1.26764723230613,-0.116307484402285));
#17840=CARTESIAN_POINT('Ctrl Pts',(-1.9817601264938,0.233436609412224,-0.042157010177434));
#17841=CARTESIAN_POINT('Ctrl Pts',(-1.26836088272398,-1.54298606011064,
0.0690687011598421));
#17842=CARTESIAN_POINT('Ctrl Pts',(0.609330548428412,-1.9001634242276,0.180294412497119));
#17843=CARTESIAN_POINT('Ctrl Pts',(1.92763134113508,-0.518030156334108,
0.291520123834394));
#17844=CARTESIAN_POINT('Ctrl Pts',(1.47944269002272,1.34021961655124,0.402745835171672));
#17845=CARTESIAN_POINT('Ctrl Pts',(-0.325091258553406,1.96930981947839,
0.513971546508948));
#17846=CARTESIAN_POINT('Ctrl Pts',(-1.8315117099918,0.793608534572646,0.625197257846224));
#17847=CARTESIAN_POINT('Ctrl Pts',(-1.65916676712527,-1.10972637539669,
0.7364229691835));
#17848=CARTESIAN_POINT('Ctrl Pts',(0.0340644505831978,-1.9957496809569,
0.847648680520777));
#17849=CARTESIAN_POINT('Ctrl Pts',(1.69605316295611,-1.05244701795271,0.958874391858054));
#17850=CARTESIAN_POINT('Ctrl Pts',(1.80338743872602,0.855593215941119,1.07010010319533));
#17851=CARTESIAN_POINT('Ctrl Pts',(0.257666548537818,1.97935179840939,1.18132581453261));
#17852=CARTESIAN_POINT('Ctrl Pts',(-1.52423826194019,1.28877211229984,1.29255152586988));
#17853=CARTESIAN_POINT('Ctrl Pts',(-1.90897240898426,-0.583146616891169,
1.40377723720716));
#17854=CARTESIAN_POINT('Ctrl Pts',(-0.543872574776452,-1.9205300179086,
1.51500294854444));
#17855=CARTESIAN_POINT('Ctrl Pts',(1.31976019388731,-1.49748707947159,1.62622865988171));
#17856=CARTESIAN_POINT('Ctrl Pts',(1.97365314915069,0.298207324296545,1.73745437121899));
#17857=CARTESIAN_POINT('Ctrl Pts',(0.818424019786662,1.82055379963935,1.84868008255626));
#17858=CARTESIAN_POINT('Ctrl Pts',(-1.08700216386266,1.6741148561284,1.95990579389354));
#17859=CARTESIAN_POINT('Ctrl Pts',(-1.99604281019441,-0.00687849795467773,
2.07113150523082));
#17860=CARTESIAN_POINT('Ctrl Pts',(-1.07543828510332,-1.68156672953773,
2.1823572165681));
#17861=CARTESIAN_POINT('Ctrl Pts',(0.830951927537738,-1.81486999562381,
2.29358292790537));
#17862=CARTESIAN_POINT('Ctrl Pts',(1.97566150203448,-0.284597659262374,
2.40480863924265));
#17863=CARTESIAN_POINT('Ctrl Pts',(1.30940816326546,1.50654719648941,2.51603435057992));
#17864=CARTESIAN_POINT('Ctrl Pts',(-0.557096136778581,1.91673631281949,
2.6272600619172));
#17865=CARTESIAN_POINT('Ctrl Pts',(-1.91294593480924,0.569975479650009,
2.73848577325448));
#17866=CARTESIAN_POINT('Ctrl Pts',(-1.51532018251605,-1.29924552753932,
2.84971148459175));
#17867=CARTESIAN_POINT('Ctrl Pts',(0.271302949066904,-1.97753101288966,
2.96093719592903));
#17868=CARTESIAN_POINT('Ctrl Pts',(1.80923996829539,-0.843139925493371,
3.0721629072663));
#17869=CARTESIAN_POINT('Ctrl Pts',(1.6887620836463,1.06410376450264,3.18338861860358));
#17870=CARTESIAN_POINT('Ctrl Pts',(0.0203036891799667,1.9959513914669,3.29461432994085));
#17871=CARTESIAN_POINT('Ctrl Pts',(-1.66676580240553,1.09823765951648,3.40584004127814));
#17872=CARTESIAN_POINT('Ctrl Pts',(-1.82601737245506,-0.806160500357498,
3.51706575261541));
#17873=CARTESIAN_POINT('Ctrl Pts',(-0.31147526217729,-1.97160273836024,
3.6282914639527));
#17874=CARTESIAN_POINT('Ctrl Pts',(1.48857635818734,-1.32980247507055,3.73951717528996));
#17875=CARTESIAN_POINT('Ctrl Pts',(1.92414495740429,0.530942915707476,3.85074288662724));
#17876=CARTESIAN_POINT('Ctrl Pts',(0.595972576764652,1.90500679384439,3.96196859796451));
#17877=CARTESIAN_POINT('Ctrl Pts',(-1.27848985988335,1.53287242622092,4.07319430930179));
#17878=CARTESIAN_POINT('Ctrl Pts',(-1.98104217115158,-0.244348343372923,
4.18442002063907));
#17879=CARTESIAN_POINT('Ctrl Pts',(-0.867699455103643,-1.79759056863662,
4.29564573197634));
#17880=CARTESIAN_POINT('Ctrl Pts',(1.04100801842068,-1.70309615192351,4.40687144331362));
#17881=CARTESIAN_POINT('Ctrl Pts',(1.99548982624636,-0.047482098928651,
4.5180971546509));
#17882=CARTESIAN_POINT('Ctrl Pts',(1.12083336301401,1.65165576596945,4.62932286598818));
#17883=CARTESIAN_POINT('Ctrl Pts',(-0.781219569426276,1.83682611665882,
4.74054857732545));
#17884=CARTESIAN_POINT('Ctrl Pts',(-1.96717833937204,0.338295099553305,
4.85177428866273));
#17885=CARTESIAN_POINT('Ctrl Pts',(-1.34995017532929,-1.47032946049761,
4.963));
#17886=CARTESIAN_POINT('Ctrl Pts',(0.504691233720185,-1.93119677026974,
5.07422571133729));
#17887=CARTESIAN_POINT('Ctrl Pts',(1.89671436244713,-0.621859146624829,
5.18545142267455));
#17888=CARTESIAN_POINT('Ctrl Pts',(1.55014040845374,1.25749708864148,5.29667713401184));
#17889=CARTESIAN_POINT('Ctrl Pts',(-0.217348443720809,1.98418595644765,
5.4079028453491));
#17890=CARTESIAN_POINT('Ctrl Pts',(-1.78560776525334,0.892098045178891,
5.5191285566864));
#17891=CARTESIAN_POINT('Ctrl Pts',(-1.71711445473246,-1.01771917087445,
5.63035426802365));
#17892=CARTESIAN_POINT('Ctrl Pts',(-0.0746515603857894,-1.99465828328709,
5.74157997936095));
#17893=CARTESIAN_POINT('Ctrl Pts',(1.63623915694148,-1.14322104099488,5.85280569069821));
#17894=CARTESIAN_POINT('Ctrl Pts',(1.84729473816909,0.756133444166813,5.96403140203549));
#17895=CARTESIAN_POINT('Ctrl Pts',(0.365051213003408,1.96238972900109,6.07525711337277));
#17896=CARTESIAN_POINT('Ctrl Pts',(-1.45180800902444,1.36984637716583,6.18648282471005));
#17897=CARTESIAN_POINT('Ctrl Pts',(-1.93789402341296,-0.478343766907873,
6.29770853604731));
#17898=CARTESIAN_POINT('Ctrl Pts',(-0.647623567773631,-1.88807435543072,
6.4089342473846));
#17899=CARTESIAN_POINT('Ctrl Pts',(1.23625811173359,-1.56711296880792,6.52015995872187));
#17900=CARTESIAN_POINT('Ctrl Pts',(1.98698654428125,0.190293095590063,6.63138567005915));
#17901=CARTESIAN_POINT('Ctrl Pts',(0.916284000920563,1.77332266653327,6.74261138139642));
#17902=CARTESIAN_POINT('Ctrl Pts',(-0.994151669926352,1.73075935608174,
6.8538370927337));
#17903=CARTESIAN_POINT('Ctrl Pts',(-1.99362816383988,0.101911912919242,
6.96506280407097));
#17904=CARTESIAN_POINT('Ctrl Pts',(-1.16507005656334,-1.62071885084899,
7.07628851540826));
#17905=CARTESIAN_POINT('Ctrl Pts',(0.730282785733831,-1.85703845110468,
7.18751422674552));
#17906=CARTESIAN_POINT('Ctrl Pts',(1.95844378280506,-0.392483452023516,
7.29873993808281));
#17907=CARTESIAN_POINT('Ctrl Pts',(1.38704085524538,1.43456736176966,7.40996564942008));
#17908=CARTESIAN_POINT('Ctrl Pts',(0.165022348489246,1.77169909665516,7.48411612364493));
#17909=CARTESIAN_POINT('Ctrl Pts',(-0.382243053164543,1.64449374968465,
7.52119136075736));
#17910=CARTESIAN_POINT('Ctrl Pts',(-0.802959149489926,1.63459616787395,
-0.0766913607573553));
#17911=CARTESIAN_POINT('Ctrl Pts',(-1.34693076903838,1.36738216262677,-0.0396161236449298));
#17912=CARTESIAN_POINT('Ctrl Pts',(-2.1376794572752,0.251802747388692,0.034534350579921));
#17913=CARTESIAN_POINT('Ctrl Pts',(-1.36815196105874,-1.66438387747571,
0.145760061917198));
#17914=CARTESIAN_POINT('Ctrl Pts',(0.657270967687777,-2.04966295523545,
0.256985773254474));
#17915=CARTESIAN_POINT('Ctrl Pts',(2.07929197083741,-0.558787316709069,
0.36821148459175));
#17916=CARTESIAN_POINT('Ctrl Pts',(1.59584109317654,1.44566433860368,0.479437195929027));
#17917=CARTESIAN_POINT('Ctrl Pts',(-0.350668527365547,2.12424959500892,
0.590662907266303));
#17918=CARTESIAN_POINT('Ctrl Pts',(-1.97560991659234,0.856047429148608,
0.70188861860358));
#17919=CARTESIAN_POINT('Ctrl Pts',(-1.7897053567994,-1.1970365354353,0.813114329940855));
#17920=CARTESIAN_POINT('Ctrl Pts',(0.0367445460535571,-2.15276967066298,
0.924340041278132));
#17921=CARTESIAN_POINT('Ctrl Pts',(1.8294938708412,-1.13525059873339,1.03556575261541));
#17922=CARTESIAN_POINT('Ctrl Pts',(1.94527290651128,0.922908891469747,1.14679146395268));
#17923=CARTESIAN_POINT('Ctrl Pts',(0.277939030194749,2.13508164868898,1.25801717528996));
#17924=CARTESIAN_POINT('Ctrl Pts',(-1.64416105510567,1.39016908895364,1.36924288662724));
#17925=CARTESIAN_POINT('Ctrl Pts',(-2.05916500621629,-0.629026957825243,
1.48046859796451));
#17926=CARTESIAN_POINT('Ctrl Pts',(-0.586662944183848,-2.07163193540842,
1.59169430930179));
#17927=CARTESIAN_POINT('Ctrl Pts',(1.42359522592366,-1.61530516459883,1.70292002063907));
#17928=CARTESIAN_POINT('Ctrl Pts',(2.12893464568308,0.32166944053191,1.81414573197634));
#17929=CARTESIAN_POINT('Ctrl Pts',(0.882815327167714,1.96378986857444,1.92537144331362));
#17930=CARTESIAN_POINT('Ctrl Pts',(-1.17252444664632,1.80582951953752,2.0365971546509));
#17931=CARTESIAN_POINT('Ctrl Pts',(-2.1530858624871,-0.00741967888950297,
2.14782286598817));
#17932=CARTESIAN_POINT('Ctrl Pts',(-1.16005075432617,-1.81386768545496,
2.25904857732545));
#17933=CARTESIAN_POINT('Ctrl Pts',(0.896328895577965,-1.95765887879382,
2.37027428866273));
#17934=CARTESIAN_POINT('Ctrl Pts',(2.13110101014124,-0.306989005208296,
2.4815));
#17935=CARTESIAN_POINT('Ctrl Pts',(1.41242872655496,1.62507810622307,2.59272571133728));
#17936=CARTESIAN_POINT('Ctrl Pts',(-0.600926898971321,2.06753975223876,
2.70395142267456));
#17937=CARTESIAN_POINT('Ctrl Pts',(-2.06345115791318,0.614819552431958,
2.81517713401183));
#17938=CARTESIAN_POINT('Ctrl Pts',(-1.63454132619476,-1.40146652314137,
2.92640284534911));
#17939=CARTESIAN_POINT('Ctrl Pts',(0.292648304487066,-2.13311760886924,
3.03762855668638));
#17940=CARTESIAN_POINT('Ctrl Pts',(1.95158589669928,-0.909475811043054,
3.14885426802366));
#17941=CARTESIAN_POINT('Ctrl Pts',(1.82162914985223,1.14782446542155,3.26007997936093));
#17942=CARTESIAN_POINT('Ctrl Pts',(0.021901126522171,2.15298725119041,3.37130569069822));
#17943=CARTESIAN_POINT('Ctrl Pts',(-1.79790226287119,1.18464391959888,3.48253140203548));
#17944=CARTESIAN_POINT('Ctrl Pts',(-1.96968329998188,-0.869586948411284,
3.59375711337277));
#17945=CARTESIAN_POINT('Ctrl Pts',(-0.335981262567754,-2.12672291432008,
3.70498282471004));
#17946=CARTESIAN_POINT('Ctrl Pts',(1.60569337274561,-1.43442760563632,3.81620853604732));
#17947=CARTESIAN_POINT('Ctrl Pts',(2.07553128820896,0.572716015788303,3.9274342473846));
#17948=CARTESIAN_POINT('Ctrl Pts',(0.642862028263319,2.05488738759502,4.03865995872187));
#17949=CARTESIAN_POINT('Ctrl Pts',(-1.37907785774386,1.65347453122567,4.14988567005915));
#17950=CARTESIAN_POINT('Ctrl Pts',(-2.13690501521948,-0.263572985985768,
4.26111138139642));
#17951=CARTESIAN_POINT('Ctrl Pts',(-0.935967615589101,-1.93901995493508,
4.3723370927337));
#17952=CARTESIAN_POINT('Ctrl Pts',(1.12291161078803,-1.83709098243517,4.48356280407097));
#17953=CARTESIAN_POINT('Ctrl Pts',(2.15248937131234,-0.0512178573537473,
4.59478851540826));
#17954=CARTESIAN_POINT('Ctrl Pts',(1.20901738969933,1.78160341113012,4.70601422674553));
#17955=CARTESIAN_POINT('Ctrl Pts',(-0.842683734957634,1.9813424458767,4.81723993808281));
#17956=CARTESIAN_POINT('Ctrl Pts',(-2.12195041602352,0.364911209557656,
4.92846564942008));
#17957=CARTESIAN_POINT('Ctrl Pts',(-1.45616047046626,-1.58601086030181,
5.03969136075736));
#17958=CARTESIAN_POINT('Ctrl Pts',(0.544398925060255,-2.08313791794051,
5.15091707209464));
#17959=CARTESIAN_POINT('Ctrl Pts',(2.04594253094371,-0.670785280865706,
5.26214278343191));
#17960=CARTESIAN_POINT('Ctrl Pts',(1.67210110988885,1.35643343411504,5.37336849476919));
#17961=CARTESIAN_POINT('Ctrl Pts',(-0.234448809924699,2.14029614472887,
5.48459420610646));
#17962=CARTESIAN_POINT('Ctrl Pts',(-1.92609437817603,0.96228581832871,5.59581991744374));
#17963=CARTESIAN_POINT('Ctrl Pts',(-1.85221220600806,-1.09779046200839,
5.70704562878101));
#17964=CARTESIAN_POINT('Ctrl Pts',(-0.0805249358672843,-2.15159240488431,
5.8182713401183));
#17965=CARTESIAN_POINT('Ctrl Pts',(1.76497386652513,-1.23316646741867,5.92949705145556));
#17966=CARTESIAN_POINT('Ctrl Pts',(1.99263470917806,0.815623903693059,6.04072276279285));
#17967=CARTESIAN_POINT('Ctrl Pts',(0.393772419001808,2.11678505121371,6.15194847413012));
#17968=CARTESIAN_POINT('Ctrl Pts',(-1.56603219295262,1.47762204968323,6.2631741854674));
#17969=CARTESIAN_POINT('Ctrl Pts',(-2.09036209218494,-0.515978513425692,
6.37439989680467));
#17970=CARTESIAN_POINT('Ctrl Pts',(-0.698576774438554,-2.03662275239797,
6.48562560814195));
#17971=CARTESIAN_POINT('Ctrl Pts',(1.33352343404865,-1.69040902370822,6.59685131947923));
#17972=CARTESIAN_POINT('Ctrl Pts',(2.14331707496162,0.205264822854154,6.70807703081651));
#17973=CARTESIAN_POINT('Ctrl Pts',(0.988374657261507,1.9128427223306,6.81930274215378));
#17974=CARTESIAN_POINT('Ctrl Pts',(-1.07236873615846,1.86693064994129,6.93052845349106));
#17975=CARTESIAN_POINT('Ctrl Pts',(-2.15048123852699,0.109930056512203,
7.04175416482834));
#17976=CARTESIAN_POINT('Ctrl Pts',(-1.25673450227717,-1.74823246626129,
7.1529798761656));
#17977=CARTESIAN_POINT('Ctrl Pts',(0.787739387928281,-2.00314503013039,
7.26420558750289));
#17978=CARTESIAN_POINT('Ctrl Pts',(2.11252864903365,-0.42336294968026,7.37543129884016));
#17979=CARTESIAN_POINT('Ctrl Pts',(1.49616934109244,1.54743509990691,7.48665701017744));
#17980=CARTESIAN_POINT('Ctrl Pts',(0.178005844219355,1.91109141452625,7.56080748440229));
#17981=CARTESIAN_POINT('Ctrl Pts',(-0.412316864948557,1.77387790748314,
7.59788272151472));
#17982=CARTESIAN_POINT('Ctrl Pts',(-0.861525859670525,1.75382131162755,
0.));
#17983=CARTESIAN_POINT('Ctrl Pts',(-1.44517400349647,1.4671170929474,0.0370752371124254));
#17984=CARTESIAN_POINT('Ctrl Pts',(-2.29359878805659,0.270168885365161,
0.111225711337276));
#17985=CARTESIAN_POINT('Ctrl Pts',(-1.46794303939349,-1.78578169484077,
0.222451422674553));
#17986=CARTESIAN_POINT('Ctrl Pts',(0.705211386947141,-2.19916248624329,
0.33367713401183));
#17987=CARTESIAN_POINT('Ctrl Pts',(2.23095260053975,-0.599544477084032,
0.444902845349104));
#17988=CARTESIAN_POINT('Ctrl Pts',(1.71223949633035,1.55110906065613,0.556128556686383));
#17989=CARTESIAN_POINT('Ctrl Pts',(-0.376245796177686,2.27918937053945,
0.667354268023658));
#17990=CARTESIAN_POINT('Ctrl Pts',(-2.11970812319287,0.918486323724569,
0.778579979360935));
#17991=CARTESIAN_POINT('Ctrl Pts',(-1.92024394647352,-1.28434669547391,
0.889805690698211));
#17992=CARTESIAN_POINT('Ctrl Pts',(0.0394246415239131,-2.30978966036907,
1.00103140203549));
#17993=CARTESIAN_POINT('Ctrl Pts',(1.96293457872629,-1.21805417951409,1.11225711337277));
#17994=CARTESIAN_POINT('Ctrl Pts',(2.08715837429654,0.990224566998375,1.22348282471004));
#17995=CARTESIAN_POINT('Ctrl Pts',(0.298211511851683,2.29081149896857,1.33470853604732));
#17996=CARTESIAN_POINT('Ctrl Pts',(-1.76408384827114,1.49156606560744,1.44593424738459));
#17997=CARTESIAN_POINT('Ctrl Pts',(-2.20935760344832,-0.674907298759319,
1.55715995872187));
#17998=CARTESIAN_POINT('Ctrl Pts',(-0.629453313591242,-2.22273385290824,
1.66838567005915));
#17999=CARTESIAN_POINT('Ctrl Pts',(1.52743025795999,-1.73312324972607,1.77961138139642));
#18000=CARTESIAN_POINT('Ctrl Pts',(2.28421614221547,0.345131556767278,1.8908370927337));
#18001=CARTESIAN_POINT('Ctrl Pts',(0.947206634548765,2.10702593750954,2.00206280407097));
#18002=CARTESIAN_POINT('Ctrl Pts',(-1.25804672942998,1.93754418294664,2.11328851540825));
#18003=CARTESIAN_POINT('Ctrl Pts',(-2.31012891477979,-0.0079608598243287,
2.22451422674552));
#18004=CARTESIAN_POINT('Ctrl Pts',(-1.24466322354901,-1.94616864137219,
2.33573993808281));
#18005=CARTESIAN_POINT('Ctrl Pts',(0.961705863618192,-2.10044776196383,
2.44696564942008));
#18006=CARTESIAN_POINT('Ctrl Pts',(2.286540518248,-0.329380351154219,2.55819136075736));
#18007=CARTESIAN_POINT('Ctrl Pts',(1.51544928984446,1.74360901595674,2.66941707209463));
#18008=CARTESIAN_POINT('Ctrl Pts',(-0.644757661164061,2.21834319165802,
2.78064278343191));
#18009=CARTESIAN_POINT('Ctrl Pts',(-2.21395638101712,0.659663625213907,
2.89186849476918));
#18010=CARTESIAN_POINT('Ctrl Pts',(-1.75376246987347,-1.50368751874342,
3.00309420610647));
#18011=CARTESIAN_POINT('Ctrl Pts',(0.313993659907229,-2.28870420484881,
3.11431991744373));
#18012=CARTESIAN_POINT('Ctrl Pts',(2.09393182510317,-0.975811696592738,
3.22554562878102));
#18013=CARTESIAN_POINT('Ctrl Pts',(1.95449621605817,1.23154516634045,3.33677134011829));
#18014=CARTESIAN_POINT('Ctrl Pts',(0.0234985638643735,2.31002311091391,
3.44799705145557));
#18015=CARTESIAN_POINT('Ctrl Pts',(-1.92903872333685,1.27105017968128,3.55922276279284));
#18016=CARTESIAN_POINT('Ctrl Pts',(-2.1133492275087,-0.93301339646507,3.67044847413012));
#18017=CARTESIAN_POINT('Ctrl Pts',(-0.360487262958215,-2.28184309027991,
3.7816741854674));
#18018=CARTESIAN_POINT('Ctrl Pts',(1.72281038730387,-1.53905273620209,3.89289989680467));
#18019=CARTESIAN_POINT('Ctrl Pts',(2.22691761901362,0.614489115869131,4.00412560814195));
#18020=CARTESIAN_POINT('Ctrl Pts',(0.689751479761988,2.20476798134566,4.11535131947922));
#18021=CARTESIAN_POINT('Ctrl Pts',(-1.47966585560437,1.77407663623043,4.22657703081651));
#18022=CARTESIAN_POINT('Ctrl Pts',(-2.29276785928738,-0.282797628598616,
4.33780274215377));
#18023=CARTESIAN_POINT('Ctrl Pts',(-1.00423577607456,-2.08044934123353,
4.44902845349105));
#18024=CARTESIAN_POINT('Ctrl Pts',(1.20481520315537,-1.97108581294683,4.56025416482834));
#18025=CARTESIAN_POINT('Ctrl Pts',(2.30948891637831,-0.0549536157788429,
4.6714798761656));
#18026=CARTESIAN_POINT('Ctrl Pts',(1.29720141638464,1.91155105629079,4.78270558750289));
#18027=CARTESIAN_POINT('Ctrl Pts',(-0.904147900488994,2.12585877509457,
4.89393129884016));
#18028=CARTESIAN_POINT('Ctrl Pts',(-2.276722492675,0.391527319562006,5.00515701017744));
#18029=CARTESIAN_POINT('Ctrl Pts',(-1.56237076560323,-1.701692260106,5.11638272151471));
#18030=CARTESIAN_POINT('Ctrl Pts',(0.584106616400323,-2.2350790656113,5.227608432852));
#18031=CARTESIAN_POINT('Ctrl Pts',(2.19517069944029,-0.71971141510658,5.33883414418926));
#18032=CARTESIAN_POINT('Ctrl Pts',(1.79406181132396,1.4553697795886,5.45005985552654));
#18033=CARTESIAN_POINT('Ctrl Pts',(-0.251549176128587,2.2964063330101,5.56128556686382));
#18034=CARTESIAN_POINT('Ctrl Pts',(-2.06658099109872,1.03247359147853,5.6725112782011));
#18035=CARTESIAN_POINT('Ctrl Pts',(-1.98730995728366,-1.17786175314234,
5.78373698953836));
#18036=CARTESIAN_POINT('Ctrl Pts',(-0.0863983113487825,-2.30852652648153,
5.89496270087566));
#18037=CARTESIAN_POINT('Ctrl Pts',(1.89370857610877,-1.32311189384246,6.00618841221292));
#18038=CARTESIAN_POINT('Ctrl Pts',(2.13797468018702,0.875114363219305,6.1174141235502));
#18039=CARTESIAN_POINT('Ctrl Pts',(0.422493625000208,2.27118037342633,6.22863983488748));
#18040=CARTESIAN_POINT('Ctrl Pts',(-1.68025637688079,1.58539772220062,6.33986554622475));
#18041=CARTESIAN_POINT('Ctrl Pts',(-2.24283016095692,-0.55361325994351,
6.45109125756204));
#18042=CARTESIAN_POINT('Ctrl Pts',(-0.749529981103475,-2.18517114936522,
6.56231696889931));
#18043=CARTESIAN_POINT('Ctrl Pts',(1.43078875636371,-1.81370507860851,6.67354268023658));
#18044=CARTESIAN_POINT('Ctrl Pts',(2.29964760564199,0.22023655011824,6.78476839157387));
#18045=CARTESIAN_POINT('Ctrl Pts',(1.06046531360245,2.05236277812793,6.89599410291113));
#18046=CARTESIAN_POINT('Ctrl Pts',(-1.15058580239056,2.00310194380083,7.00721981424842));
#18047=CARTESIAN_POINT('Ctrl Pts',(-2.30733431321409,0.117948200105168,
7.11844552558569));
#18048=CARTESIAN_POINT('Ctrl Pts',(-1.34839894799099,-1.87574608167359,
7.22967123692297));
#18049=CARTESIAN_POINT('Ctrl Pts',(0.845195990122731,-2.1492516091561,7.34089694826023));
#18050=CARTESIAN_POINT('Ctrl Pts',(2.26661351526224,-0.454242447337005,
7.45212265959753));
#18051=CARTESIAN_POINT('Ctrl Pts',(1.60529782693949,1.66030283804416,7.56334837093479));
#18052=CARTESIAN_POINT('Ctrl Pts',(0.190989339949464,2.05048373239734,7.63749884515964));
#18053=CARTESIAN_POINT('Ctrl Pts',(-0.442390676732572,1.90326206528163,
7.67457408227207));
#18054=CARTESIAN_POINT('Ctrl Pts',(-1.95381346134878,-0.0017935399644829,
6.42413030787577));
#18055=CARTESIAN_POINT('Ctrl Pts',(-1.9552538907035,-0.159408210813097,
6.43311729110453));
#18056=CARTESIAN_POINT('Ctrl Pts',(-1.93778561972322,-0.316707681574419,
6.44210427433328));
#18057=CARTESIAN_POINT('Ctrl Pts',(-1.90018450030199,-0.469037744489771,
6.45109125756203));
#18058=CARTESIAN_POINT('Ctrl Pts',(-1.7450634343391,-1.09746588975075,6.48816649467446));
#18059=CARTESIAN_POINT('Ctrl Pts',(-1.24729670772129,-1.64131851955799,
6.52524173178688));
#18060=CARTESIAN_POINT('Ctrl Pts',(-0.635026888167849,-1.85133382266882,
6.56231696889931));
#18061=CARTESIAN_POINT('Ctrl Pts',(-0.02275706861441,-2.06134912577965,
6.59939220601173));
#18062=CARTESIAN_POINT('Ctrl Pts',(0.704015843874659,-1.93752710219408,
6.63646744312416));
#18063=CARTESIAN_POINT('Ctrl Pts',(1.21221210833224,-1.53662581894683,6.67354268023658));
#18064=CARTESIAN_POINT('Ctrl Pts',(1.7204083727898,-1.1357245356996,6.71061791734901));
#18065=CARTESIAN_POINT('Ctrl Pts',(2.01002798921589,-0.457743992790703,
6.74769315446144));
#18066=CARTESIAN_POINT('Ctrl Pts',(1.94830741542236,0.186600649998693,6.78476839157386));
#18067=CARTESIAN_POINT('Ctrl Pts',(1.88658684162883,0.830945292788112,6.82184362868628));
#18068=CARTESIAN_POINT('Ctrl Pts',(1.47352607761564,1.44165403545803,6.85891886579871));
#18069=CARTESIAN_POINT('Ctrl Pts',(0.898487176276873,1.73879826773846,6.89599410291113));
#18070=CARTESIAN_POINT('Ctrl Pts',(0.323448274938114,2.0359425000189,6.93306934002356));
#18071=CARTESIAN_POINT('Ctrl Pts',(-0.413568763726226,2.01952222190986,
6.97014457713599));
#18072=CARTESIAN_POINT('Ctrl Pts',(-0.974868701528982,1.69711979223941,
7.00721981424841));
#18073=CARTESIAN_POINT('Ctrl Pts',(-1.17057269468519,1.58471029663753,7.02014654283228));
#18074=CARTESIAN_POINT('Ctrl Pts',(-1.344915597571,1.43510400955329,7.03307327141614));
#18075=CARTESIAN_POINT('Ctrl Pts',(-1.49039960333529,1.260503289177,7.046));
#18076=CARTESIAN_POINT('Ctrl Pts',(-0.905552056217064,-1.26793026328003,
2.94902990916057E-17));
#18077=CARTESIAN_POINT('Ctrl Pts',(-0.937134822631023,-1.25104249355971,
4.75162406228688E-17));
#18078=CARTESIAN_POINT('Ctrl Pts',(-0.968036761240596,-1.23301924856148,
-1.58634398933136E-16));
#18079=CARTESIAN_POINT('Ctrl Pts',(-0.998189477963827,-1.21387418528302,
-1.99493199737333E-16));
#18080=CARTESIAN_POINT('Ctrl Pts',(-1.04824220989901,-1.18209387411058,
-2.7512401071258E-16));
#18081=CARTESIAN_POINT('Ctrl Pts',(-1.09623172292828,-1.14722531738451,
-1.13947733410607E-16));
#18082=CARTESIAN_POINT('Ctrl Pts',(-1.14207949782356,-1.10958932626875,
-2.28983498828939E-16));
#18083=CARTESIAN_POINT('Ctrl Pts',(-1.16812476791348,-1.08820901815237,
-2.94333182366767E-16));
#18084=CARTESIAN_POINT('Ctrl Pts',(-1.19347860393222,-1.06593466358557,
-2.59231987339497E-16));
#18085=CARTESIAN_POINT('Ctrl Pts',(-1.21812392229353,-1.04281835170969,
-2.1163626406917E-16));
#18086=CARTESIAN_POINT('Ctrl Pts',(-1.23207453972119,-1.02973323677667,
-1.84694444255666E-16));
#18087=CARTESIAN_POINT('Ctrl Pts',(-1.24580226168736,-1.01637377846959,
3.24804729171387E-17));
#18088=CARTESIAN_POINT('Ctrl Pts',(-1.2592797890629,-1.00277371885107,1.38777878078145E-17));
#18089=CARTESIAN_POINT('Ctrl Pts',(-1.30315654392119,-0.95849805423447,
-4.66841707402696E-17));
#18090=CARTESIAN_POINT('Ctrl Pts',(-1.34442524303116,-0.911639949761556,
-4.44200463634023E-16));
#18091=CARTESIAN_POINT('Ctrl Pts',(-1.38299703120573,-0.862548384977714,
-4.09394740330526E-16));
#18092=CARTESIAN_POINT('Ctrl Pts',(-1.41261207961662,-0.824856353147081,
-3.82671240347992E-16));
#18093=CARTESIAN_POINT('Ctrl Pts',(-1.44063702556457,-0.785846462927244,
-3.12176496943412E-16));
#18094=CARTESIAN_POINT('Ctrl Pts',(-1.46702161869435,-0.745658482546257,
-3.67761376907083E-16));
#18095=CARTESIAN_POINT('Ctrl Pts',(-1.48012065014873,-0.725706550124602,
-3.9535733366299E-16));
#18096=CARTESIAN_POINT('Ctrl Pts',(-1.4928152185087,-0.705464023789787,
-1.55640291167757E-16));
#18097=CARTESIAN_POINT('Ctrl Pts',(-1.50509817356396,-0.68494682789941,
-1.17961196366423E-16));
#18098=CARTESIAN_POINT('Ctrl Pts',(-1.5112932288107,-0.674598734832467,
-9.89572943826601E-17));
#18099=CARTESIAN_POINT('Ctrl Pts',(-1.51737856906155,-0.664189090325049,
-2.93080070452884E-16));
#18100=CARTESIAN_POINT('Ctrl Pts',(-1.52335311621856,-0.653721302282831,
-2.77555756156289E-16));
#18101=CARTESIAN_POINT('Ctrl Pts',(-1.55547318924941,-0.597444883744102,
-1.94094684403748E-16));
#18102=CARTESIAN_POINT('Ctrl Pts',(-1.58439860819566,-0.539482552118629,
-3.31420483543467E-16));
#18103=CARTESIAN_POINT('Ctrl Pts',(-1.61003533926912,-0.480187572841947,
-3.19189119579733E-16));
#18104=CARTESIAN_POINT('Ctrl Pts',(-1.63616747730804,-0.419746770969312,
-3.06721395415186E-16));
#18105=CARTESIAN_POINT('Ctrl Pts',(-1.65888335052524,-0.357920523309995,
-2.80209762252872E-16));
#18106=CARTESIAN_POINT('Ctrl Pts',(-1.67804895967927,-0.295042072125015,
-1.66533453693773E-16));
#18107=CARTESIAN_POINT('Ctrl Pts',(-1.69039160882678,-0.254548359888778,
-9.33259296514283E-17));
#18108=CARTESIAN_POINT('Ctrl Pts',(-1.70126111007635,-0.213617460141972,
-2.30505991696603E-16));
#18109=CARTESIAN_POINT('Ctrl Pts',(-1.71061208520917,-0.172332131165316,
-2.91433543964104E-16));
#18110=CARTESIAN_POINT('Ctrl Pts',(-1.715816487101,-0.149354266164202,-3.2534353343379E-16));
#18111=CARTESIAN_POINT('Ctrl Pts',(-1.72055036402814,-0.126266539334649,
-1.00298932279788E-16));
#18112=CARTESIAN_POINT('Ctrl Pts',(-1.72480472543126,-0.103082789841687,
-9.71445146547012E-17));
#18113=CARTESIAN_POINT('Ctrl Pts',(-1.72695538876364,-0.0913629486676286,
-9.55498945276206E-17));
#18114=CARTESIAN_POINT('Ctrl Pts',(-1.72898375858757,-0.07961694527504,
-1.96680959500023E-16));
#18115=CARTESIAN_POINT('Ctrl Pts',(-1.73088777000182,-0.0678516147389183,
-1.94289029309402E-16));
#18116=CARTESIAN_POINT('Ctrl Pts',(-1.74172080812434,-0.000911745960731708,
-1.80679934979654E-16));
#18117=CARTESIAN_POINT('Ctrl Pts',(-1.74848760095285,0.0663732156671881,
-2.27318435210151E-17));
#18118=CARTESIAN_POINT('Ctrl Pts',(-1.75106859893149,0.133645381706535,
-4.16333634234434E-17));
#18119=CARTESIAN_POINT('Ctrl Pts',(-1.75197360252239,0.157233758116401,
-4.82610103750263E-17));
#18120=CARTESIAN_POINT('Ctrl Pts',(-1.75236359562623,0.180820850215305,
-8.28170566717793E-17));
#18121=CARTESIAN_POINT('Ctrl Pts',(-1.75223214201128,0.204392038445102,
-5.55111512312578E-17));
#18122=CARTESIAN_POINT('Ctrl Pts',(-1.75187057279805,0.269225675666801,
2.10533692500149E-17));
#18123=CARTESIAN_POINT('Ctrl Pts',(-1.74756789056806,0.333938320850628,
-1.60420900056E-17));
#18124=CARTESIAN_POINT('Ctrl Pts',(-1.73954116331082,0.398294466418659,
0.));
#18125=CARTESIAN_POINT('Ctrl Pts',(-1.73091740426649,0.467437452671242,
1.72353082822116E-17));
#18126=CARTESIAN_POINT('Ctrl Pts',(-1.71799540177027,0.536169874708505,
-4.36478159584899E-17));
#18127=CARTESIAN_POINT('Ctrl Pts',(-1.70098034075862,0.604204029641736,
8.32667268468867E-17));
#18128=CARTESIAN_POINT('Ctrl Pts',(-1.69824130486499,0.615155973465351,
1.03697067233541E-16));
#18129=CARTESIAN_POINT('Ctrl Pts',(-1.69539827041295,0.626080961021427,
1.29813171089747E-16));
#18130=CARTESIAN_POINT('Ctrl Pts',(-1.69245305315959,0.636975805303662,
1.11022302462516E-16));
#18131=CARTESIAN_POINT('Ctrl Pts',(-1.67473398681781,0.702521553550295,
-2.02764230671151E-18));
#18132=CARTESIAN_POINT('Ctrl Pts',(-1.65331496860816,0.766998932259627,
-2.57263159617093E-16));
#18133=CARTESIAN_POINT('Ctrl Pts',(-1.62845169327078,0.83015154980978,-1.94289029309402E-16));
#18134=CARTESIAN_POINT('Ctrl Pts',(-1.60307671281799,0.894603896257815,
-1.30018843507023E-16));
#18135=CARTESIAN_POINT('Ctrl Pts',(-1.57411406965586,0.957677277748301,
-1.42237185085071E-16));
#18136=CARTESIAN_POINT('Ctrl Pts',(-1.54178048300264,1.01910167818773,-5.55111512312578E-17));
#18137=CARTESIAN_POINT('Ctrl Pts',(-1.50922784853364,1.08094220569947,3.18024186880875E-17));
#18138=CARTESIAN_POINT('Ctrl Pts',(-1.47325811155629,1.14111231916335,-1.86023089836484E-16));
#18139=CARTESIAN_POINT('Ctrl Pts',(-1.43404118681899,1.19932479720781,-1.66533453693773E-16));
#18140=CARTESIAN_POINT('Ctrl Pts',(-1.42513259519695,1.21254845504633,-1.62106150675484E-16));
#18141=CARTESIAN_POINT('Ctrl Pts',(-1.41605624454103,1.22567101155683,-3.77067070771252E-16));
#18142=CARTESIAN_POINT('Ctrl Pts',(-1.40681378949184,1.23868893327645,-3.88578058618805E-16));
#18143=CARTESIAN_POINT('Ctrl Pts',(-1.40005105796202,1.24821418486786,-3.97000682266051E-16));
#18144=CARTESIAN_POINT('Ctrl Pts',(-1.39319940015811,1.25768325768832,-4.06719094166719E-16));
#18145=CARTESIAN_POINT('Ctrl Pts',(-1.3862680939899,1.26708342641975,-3.88578058618805E-16));
#18146=CARTESIAN_POINT('Ctrl Pts',(-1.34342259960335,1.32519006127916,-2.76440228046676E-16));
#18147=CARTESIAN_POINT('Ctrl Pts',(-1.2974598126633,1.38077597290076,-1.69458509682717E-16));
#18148=CARTESIAN_POINT('Ctrl Pts',(-1.24862081372783,1.43356038861728,-1.94289029309402E-16));
#18149=CARTESIAN_POINT('Ctrl Pts',(-1.19966911793571,1.48646660530969,-2.19176845800727E-16));
#18150=CARTESIAN_POINT('Ctrl Pts',(-1.14782748930566,1.53655939185262,-1.74330404157582E-16));
#18151=CARTESIAN_POINT('Ctrl Pts',(-1.09328907277386,1.5835398262669,-5.55111512312578E-17));
#18152=CARTESIAN_POINT('Ctrl Pts',(-1.03991703070208,1.62951552342795,6.07669985463979E-17));
#18153=CARTESIAN_POINT('Ctrl Pts',(-0.983961746585148,1.67251142482066,
1.56834561468643E-16));
#18154=CARTESIAN_POINT('Ctrl Pts',(-0.925564466602708,1.71221823957964,
2.22044604925031E-16));
#18155=CARTESIAN_POINT('Ctrl Pts',(-0.904533489913129,1.72651810244765,
2.45529104618684E-16));
#18156=CARTESIAN_POINT('Ctrl Pts',(-0.883185451447723,1.74039103644132,
-1.04689938393391E-17));
#18157=CARTESIAN_POINT('Ctrl Pts',(-0.861525859670525,1.75382131162755,
0.));
#18158=CARTESIAN_POINT('Origin',(0.,0.,0.));
#18159=CARTESIAN_POINT('Origin',(-0.866025403784439,-1.5,-4.));
#18160=CARTESIAN_POINT('',(-0.866025403784439,-1.5,-4.));
#18161=CARTESIAN_POINT('',(0.866025403784439,-1.5,-4.));
#18162=CARTESIAN_POINT('',(-0.43301270189222,-1.5,-4.));
#18163=CARTESIAN_POINT('',(-0.866025403784439,-1.5,-2.));
#18164=CARTESIAN_POINT('',(-0.866025403784439,-1.5,-4.));
#18165=CARTESIAN_POINT('',(0.866025403784439,-1.5,-2.));
#18166=CARTESIAN_POINT('',(-0.866025403784439,-1.5,-2.));
#18167=CARTESIAN_POINT('',(0.866025403784439,-1.5,-4.));
#18168=CARTESIAN_POINT('Origin',(-1.73205080756888,2.12115047744981E-16,
-4.));
#18169=CARTESIAN_POINT('',(-1.73205080756888,2.12115047744981E-16,-4.));
#18170=CARTESIAN_POINT('',(-1.51554445662277,-0.375,-4.));
#18171=CARTESIAN_POINT('',(-1.73205080756888,2.77555756156289E-16,-2.));
#18172=CARTESIAN_POINT('',(-1.73205080756888,2.12115047744981E-16,-4.));
#18173=CARTESIAN_POINT('',(-1.73205080756888,2.12115047744981E-16,-2.));
#18174=CARTESIAN_POINT('Origin',(-0.866025403784438,1.5,-4.));
#18175=CARTESIAN_POINT('',(-0.866025403784438,1.5,-4.));
#18176=CARTESIAN_POINT('',(-1.08253175473055,1.125,-4.));
#18177=CARTESIAN_POINT('',(-0.866025403784438,1.5,-2.));
#18178=CARTESIAN_POINT('',(-0.866025403784438,1.5,-4.));
#18179=CARTESIAN_POINT('',(-0.866025403784438,1.5,-2.));
#18180=CARTESIAN_POINT('Origin',(0.866025403784439,1.5,-4.));
#18181=CARTESIAN_POINT('',(0.866025403784439,1.5,-4.));
#18182=CARTESIAN_POINT('',(0.43301270189222,1.5,-4.));
#18183=CARTESIAN_POINT('',(0.866025403784439,1.5,-2.));
#18184=CARTESIAN_POINT('',(0.866025403784439,1.5,-4.));
#18185=CARTESIAN_POINT('',(0.866025403784439,1.5,-2.));
#18186=CARTESIAN_POINT('Origin',(1.73205080756888,0.,-4.));
#18187=CARTESIAN_POINT('',(1.73205080756888,0.,-4.));
#18188=CARTESIAN_POINT('',(1.51554445662277,0.375,-4.));
#18189=CARTESIAN_POINT('',(1.73205080756888,0.,-2.));
#18190=CARTESIAN_POINT('',(1.73205080756888,0.,-4.));
#18191=CARTESIAN_POINT('',(1.73205080756888,0.,-2.));
#18192=CARTESIAN_POINT('Origin',(0.866025403784439,-1.5,-4.));
#18193=CARTESIAN_POINT('',(1.08253175473055,-1.125,-4.));
#18194=CARTESIAN_POINT('',(0.866025403784439,-1.5,-2.));
#18195=CARTESIAN_POINT('Origin',(0.,2.77555756156289E-16,-2.));
#18196=CARTESIAN_POINT('Origin',(0.,0.,0.));
#18197=CARTESIAN_POINT('',(-3.5,-4.28626379701574E-16,0.));
#18198=CARTESIAN_POINT('Origin',(0.,0.,0.));
#18199=CARTESIAN_POINT('Origin',(0.,0.,-4.));
#18200=CARTESIAN_POINT('',(-3.5,-4.28626379701574E-16,-4.));
#18201=CARTESIAN_POINT('',(-3.5,-4.28626379701574E-16,-4.));
#18202=CARTESIAN_POINT('Origin',(0.,0.,-4.));
#18203=CARTESIAN_POINT('Origin',(0.,0.,-4.));
#18204=CARTESIAN_POINT('Origin',(0.,0.,8.));
#18205=CARTESIAN_POINT('',(0.,0.,0.));
#18206=CARTESIAN_POINT('Origin',(0.,0.,0.));
#18207=CARTESIAN_POINT('',(-2.94490570994055,0.00214417779480537,0.322176117089595));
#18208=CARTESIAN_POINT('',(-2.94453111094736,0.00313617179185542,0.177823882910391));
#18209=CARTESIAN_POINT('',(-2.942,-3.60291088309151E-16,0.));
#18210=CARTESIAN_POINT('',(1.28892185405323,2.64462557919718,0.));
#18211=CARTESIAN_POINT('Ctrl Pts',(-2.94490570994055,0.00214417779480537,
0.322176117089595));
#18212=CARTESIAN_POINT('Ctrl Pts',(-2.94584715833611,0.124808428590093,
0.315520895872749));
#18213=CARTESIAN_POINT('Ctrl Pts',(-2.93884007386573,0.247358426874668,
0.308865674655903));
#18214=CARTESIAN_POINT('Ctrl Pts',(-2.92351947045398,0.368852411761562,
0.302210453439057));
#18215=CARTESIAN_POINT('Ctrl Pts',(-2.80238513102988,1.32946037267173,0.249590083068687));
#18216=CARTESIAN_POINT('Ctrl Pts',(-2.16153286152783,2.22405187279705,0.196969712698316));
#18217=CARTESIAN_POINT('Ctrl Pts',(-1.29099252632988,2.64857098947325,0.144349342327946));
#18218=CARTESIAN_POINT('Ctrl Pts',(-0.494964144347145,3.03675434170317,
0.0962328948852971));
#18219=CARTESIAN_POINT('Ctrl Pts',(0.493115753268411,3.03189109212113,0.0481164474426485));
#18220=CARTESIAN_POINT('Ctrl Pts',(1.29200104020318,2.64812001020929,-1.63834222883338E-16));
#18221=CARTESIAN_POINT('',(-1.28892185405328,2.64462557919715,0.));
#18222=CARTESIAN_POINT('Origin',(0.,0.,0.));
#18223=CARTESIAN_POINT('Ctrl Pts',(-1.28892185405328,2.64462557919715,2.08166817117217E-15));
#18224=CARTESIAN_POINT('Ctrl Pts',(-2.16403831185616,2.21811653527939,0.0526649636666859));
#18225=CARTESIAN_POINT('Ctrl Pts',(-2.80357657272064,1.32706756586464,0.10532992733337));
#18226=CARTESIAN_POINT('Ctrl Pts',(-2.92355402589586,0.366959843828546,
0.157994891000053));
#18227=CARTESIAN_POINT('Ctrl Pts',(-2.93861167702227,0.246462477535227,
0.164604554970166));
#18228=CARTESIAN_POINT('Ctrl Pts',(-2.94548559297357,0.124877349165528,
0.171214218940278));
#18229=CARTESIAN_POINT('Ctrl Pts',(-2.94453111094736,0.00313617179185542,
0.177823882910391));
#18230=CARTESIAN_POINT('Origin',(0.,0.,0.));
#18231=CARTESIAN_POINT('',(-2.93741501075088,0.000605053430647595,1.3221761170896));
#18232=CARTESIAN_POINT('',(-2.93743260967528,0.000720687897601403,1.17782388291039));
#18233=CARTESIAN_POINT('',(-2.942,-3.60291088309151E-16,0.));
#18234=CARTESIAN_POINT('Ctrl Pts',(-2.93741501075088,0.000605053430647595,
1.3221761170896));
#18235=CARTESIAN_POINT('Ctrl Pts',(-2.9382479568139,0.450815163107398,1.29790978476164));
#18236=CARTESIAN_POINT('Ctrl Pts',(-2.84099804532476,0.900683451883265,
1.27364345243368));
#18237=CARTESIAN_POINT('Ctrl Pts',(-2.64378204823906,1.30134356458571,1.24937712010572));
#18238=CARTESIAN_POINT('Ctrl Pts',(-2.21612867774369,2.17015567999336,1.19675674973535));
#18239=CARTESIAN_POINT('Ctrl Pts',(-1.31841648749453,2.80758195059898,1.14413637936498));
#18240=CARTESIAN_POINT('Ctrl Pts',(-0.357192829781819,2.92497002089294,
1.09151600899461));
#18241=CARTESIAN_POINT('Ctrl Pts',(0.604030827930888,3.04235809118689,1.03889563862424));
#18242=CARTESIAN_POINT('Ctrl Pts',(1.62876595310715,2.63970796116917,0.986275268253872));
#18243=CARTESIAN_POINT('Ctrl Pts',(2.25292793158662,1.89932766827126,0.933654897883501));
#18244=CARTESIAN_POINT('Ctrl Pts',(2.8770899100661,1.15894737537334,0.881034527513131));
#18245=CARTESIAN_POINT('Ctrl Pts',(3.1006787418488,0.0808369195952267,0.828414157142761));
#18246=CARTESIAN_POINT('Ctrl Pts',(2.82245137682484,-0.846673957408537,
0.775793786772391));
#18247=CARTESIAN_POINT('Ctrl Pts',(2.54422401180089,-1.7741848344123,0.72317341640202));
#18248=CARTESIAN_POINT('Ctrl Pts',(1.76418044997028,-2.55109613264171,0.67055304603165));
#18249=CARTESIAN_POINT('Ctrl Pts',(0.835554749603298,-2.82571794203434,
0.617932675661279));
#18250=CARTESIAN_POINT('Ctrl Pts',(-0.0930709507636752,-3.10033975142697,
0.565312305290909));
#18251=CARTESIAN_POINT('Ctrl Pts',(-1.17027878966702,-2.87267207198282,
0.512691934920538));
#18252=CARTESIAN_POINT('Ctrl Pts',(-1.90817450444562,-2.24552602141323,
0.460071564550168));
#18253=CARTESIAN_POINT('Ctrl Pts',(-2.55274401908064,-1.69769898118953,
0.414106415396644));
#18254=CARTESIAN_POINT('Ctrl Pts',(-2.93840347440061,-0.845052391620324,
0.368141266243119));
#18255=CARTESIAN_POINT('Ctrl Pts',(-2.94490570994055,0.00214417779480537,
0.322176117089595));
#18256=CARTESIAN_POINT('Ctrl Pts',(-2.94453111094736,0.00313617179185542,
0.177823882910391));
#18257=CARTESIAN_POINT('Ctrl Pts',(-2.93788040132423,-0.845140901703999,
0.223879182606963));
#18258=CARTESIAN_POINT('Ctrl Pts',(-2.55115114237882,-1.7009943502416,0.269934482303535));
#18259=CARTESIAN_POINT('Ctrl Pts',(-1.90455354763271,-2.24922658650796,
0.315989782000107));
#18260=CARTESIAN_POINT('Ctrl Pts',(-1.16515897070839,-2.87613882015091,
0.368654745666792));
#18261=CARTESIAN_POINT('Ctrl Pts',(-0.0859531713737992,-3.10079681277935,
0.421319709333476));
#18262=CARTESIAN_POINT('Ctrl Pts',(0.842833952810694,-2.82335342322726,
0.473984673000161));
#18263=CARTESIAN_POINT('Ctrl Pts',(1.77162107699519,-2.54591003367518,0.526649636666845));
#18264=CARTESIAN_POINT('Ctrl Pts',(2.54998952602959,-1.76636526194256,0.57931460033353));
#18265=CARTESIAN_POINT('Ctrl Pts',(2.82526196809064,-0.837265996441287,
0.631979564000215));
#18266=CARTESIAN_POINT('Ctrl Pts',(3.1005344101517,0.0918332690599885,0.684644527666899));
#18267=CARTESIAN_POINT('Ctrl Pts',(2.87271084523941,1.17048702832993,0.737309491333584));
#18268=CARTESIAN_POINT('Ctrl Pts',(2.2449320231631,1.90890163868963,0.789974455000268));
#18269=CARTESIAN_POINT('Ctrl Pts',(1.61715320108678,2.64731624904933,0.842639418666953));
#18270=CARTESIAN_POINT('Ctrl Pts',(0.589419121846451,3.0454917104988,0.895304382333637));
#18271=CARTESIAN_POINT('Ctrl Pts',(-0.37200976733393,2.9231058378395,0.947969346000322));
#18272=CARTESIAN_POINT('Ctrl Pts',(-1.33343865651431,2.8007199651802,1.00063430966701));
#18273=CARTESIAN_POINT('Ctrl Pts',(-2.22856235563474,2.15777275841214,1.05329927333369));
#18274=CARTESIAN_POINT('Ctrl Pts',(-2.6514251854394,1.28574400496261,1.10596423700038));
#18275=CARTESIAN_POINT('Ctrl Pts',(-2.8437527539192,0.889125626674557,1.12991745230371));
#18276=CARTESIAN_POINT('Ctrl Pts',(-2.93838674329414,0.445118617110292,
1.15387066760705));
#18277=CARTESIAN_POINT('Ctrl Pts',(-2.93743260967528,0.000720687897601403,
1.17782388291039));
#18278=CARTESIAN_POINT('Origin',(0.,0.,0.));
#18279=CARTESIAN_POINT('',(-2.94283216929169,-0.00254059509496668,2.3221761170896));
#18280=CARTESIAN_POINT('',(-2.94249560619114,-0.00258942729680482,2.17782388291039));
#18281=CARTESIAN_POINT('',(-2.942,-3.60291088309151E-16,0.));
#18282=CARTESIAN_POINT('Ctrl Pts',(-2.94283216929169,-0.00254059509496668,
2.3221761170896));
#18283=CARTESIAN_POINT('Ctrl Pts',(-2.93583836831966,0.770783310741536,
2.28029867365053));
#18284=CARTESIAN_POINT('Ctrl Pts',(-2.62244249954969,1.54912568223824,2.23842123021146));
#18285=CARTESIAN_POINT('Ctrl Pts',(-2.07534059520784,2.09189740289201,2.19654378677239));
#18286=CARTESIAN_POINT('Ctrl Pts',(-1.38788924974329,2.77390773164861,2.14392341640202));
#18287=CARTESIAN_POINT('Ctrl Pts',(-0.331445515483537,3.08398167899393,
2.09130304603165));
#18288=CARTESIAN_POINT('Ctrl Pts',(0.615553755286461,2.88169496582278,2.03868267566128));
#18289=CARTESIAN_POINT('Ctrl Pts',(1.56255302605646,2.67940825265162,1.98606230529091));
#18290=CARTESIAN_POINT('Ctrl Pts',(2.40010783333669,1.96476087896396,1.93344193492054));
#18291=CARTESIAN_POINT('Ctrl Pts',(2.74891040156469,1.06139789331815,1.88082156455017));
#18292=CARTESIAN_POINT('Ctrl Pts',(3.09771296979268,0.158034907672333,1.8282011941798));
#18293=CARTESIAN_POINT('Ctrl Pts',(2.95776329896845,-0.934043689931643,
1.77558082380943));
#18294=CARTESIAN_POINT('Ctrl Pts',(2.39244139669332,-1.72026117030417,1.72296045343906));
#18295=CARTESIAN_POINT('Ctrl Pts',(1.82711949441818,-2.50647865067671,1.67034008306869));
#18296=CARTESIAN_POINT('Ctrl Pts',(0.836425360692154,-2.9868350138178,1.61771971269832));
#18297=CARTESIAN_POINT('Ctrl Pts',(-0.130980997368149,-2.9437920444354,
1.56509934232795));
#18298=CARTESIAN_POINT('Ctrl Pts',(-1.09838735542844,-2.90074907505299,
1.51247897195758));
#18299=CARTESIAN_POINT('Ctrl Pts',(-2.04250593782301,-2.33430677314711,
1.45985860158721));
#18300=CARTESIAN_POINT('Ctrl Pts',(-2.5357679536495,-1.50098664208934,1.40723823121684));
#18301=CARTESIAN_POINT('Ctrl Pts',(-2.80155798635321,-1.05195919262036,
1.37888419317442));
#18302=CARTESIAN_POINT('Ctrl Pts',(-2.93644175348072,-0.525443729069001,
1.35053015513201));
#18303=CARTESIAN_POINT('Ctrl Pts',(-2.93741501075088,0.000605053430647595,
1.3221761170896));
#18304=CARTESIAN_POINT('Ctrl Pts',(-2.93743260967528,0.000720687897601403,
1.17782388291039));
#18305=CARTESIAN_POINT('Ctrl Pts',(-2.93628892837727,-0.53196109845813,
1.20653563127374));
#18306=CARTESIAN_POINT('Ctrl Pts',(-2.79780571115684,-1.06520455211536,
1.23524737963708));
#18307=CARTESIAN_POINT('Ctrl Pts',(-2.52560900690579,-1.51806949138664,
1.26395912800043));
#18308=CARTESIAN_POINT('Ctrl Pts',(-2.02632803807862,-2.34874393415536,
1.31662409166711));
#18309=CARTESIAN_POINT('Ctrl Pts',(-1.07716413993538,-2.9089825195618,1.3692890553338));
#18310=CARTESIAN_POINT('Ctrl Pts',(-0.108652539320438,-2.94471329972367,
1.42195401900048));
#18311=CARTESIAN_POINT('Ctrl Pts',(0.85985906129451,-2.98044407988555,1.47461898266717));
#18312=CARTESIAN_POINT('Ctrl Pts',(1.84771836438116,-2.49166705480286,1.52728394633385));
#18313=CARTESIAN_POINT('Ctrl Pts',(2.40686102399513,-1.70005997098112,1.57994891000054));
#18314=CARTESIAN_POINT('Ctrl Pts',(2.9660036836091,-0.908452887159384,1.63261387366722));
#18315=CARTESIAN_POINT('Ctrl Pts',(3.09642969975039,0.185984255401396,1.68527883733391));
#18316=CARTESIAN_POINT('Ctrl Pts',(2.73897659148843,1.08682694396802,1.73794380100059));
#18317=CARTESIAN_POINT('Ctrl Pts',(2.38152348322647,1.98766963253464,1.79060876466727));
#18318=CARTESIAN_POINT('Ctrl Pts',(1.53619125056127,2.69491786710711,1.84327372833396));
#18319=CARTESIAN_POINT('Ctrl Pts',(0.586406744725485,2.88778465426983,1.89593869200064));
#18320=CARTESIAN_POINT('Ctrl Pts',(-0.363377761110303,3.08065144143255,
1.94860365566733));
#18321=CARTESIAN_POINT('Ctrl Pts',(-1.41761454011667,2.75913678118554,2.00126861933401));
#18322=CARTESIAN_POINT('Ctrl Pts',(-2.09812527093809,2.0690698668059,2.0539335830007));
#18323=CARTESIAN_POINT('Ctrl Pts',(-2.63174175688638,1.52795998382732,2.09523034963726));
#18324=CARTESIAN_POINT('Ctrl Pts',(-2.93556254699721,0.76023565397735,2.13652711627383));
#18325=CARTESIAN_POINT('Ctrl Pts',(-2.94249560619114,-0.00258942729680482,
2.17782388291039));
#18326=CARTESIAN_POINT('Origin',(0.,0.,0.));
#18327=CARTESIAN_POINT('',(-2.94484294150901,0.00199174253909633,3.3221761170896));
#18328=CARTESIAN_POINT('',(-2.94526037616607,0.00180040430511289,3.17782388291039));
#18329=CARTESIAN_POINT('',(-2.942,-3.60291088309151E-16,0.));
#18330=CARTESIAN_POINT('Ctrl Pts',(-2.94484294150901,0.00199174253909633,
3.3221761170896));
#18331=CARTESIAN_POINT('Ctrl Pts',(-2.94583002736539,0.128597483532049,
3.31530793290979));
#18332=CARTESIAN_POINT('Ctrl Pts',(-2.93836342958051,0.255086036799256,
3.30843974872998));
#18333=CARTESIAN_POINT('Ctrl Pts',(-2.92204585589404,0.380422278131109,
3.30157156455017));
#18334=CARTESIAN_POINT('Ctrl Pts',(-2.79702929424561,1.34068182665933,3.2489511941798));
#18335=CARTESIAN_POINT('Ctrl Pts',(-2.15247739366928,2.23330287085301,3.19633082380943));
#18336=CARTESIAN_POINT('Ctrl Pts',(-1.28029158434589,2.65403966800756,3.14371045343906));
#18337=CARTESIAN_POINT('Ctrl Pts',(-0.4081057750225,3.0747764651621,3.09109008306869));
#18338=CARTESIAN_POINT('Ctrl Pts',(0.69171394304795,3.0236290152775,3.03846971269832));
#18339=CARTESIAN_POINT('Ctrl Pts',(1.5210867384019,2.5237607280468,2.98584934232795));
#18340=CARTESIAN_POINT('Ctrl Pts',(2.35045953375586,2.0238924408161,2.93322897195758));
#18341=CARTESIAN_POINT('Ctrl Pts',(2.90938540639331,1.07530331623929,2.8806086015872));
#18342=CARTESIAN_POINT('Ctrl Pts',(2.94474080948057,0.107585617606989,2.82798823121683));
#18343=CARTESIAN_POINT('Ctrl Pts',(2.98009621256783,-0.860132081025304,
2.77536786084646));
#18344=CARTESIAN_POINT('Ctrl Pts',(2.49188114610491,-1.84697835371309,2.7227474904761));
#18345=CARTESIAN_POINT('Ctrl Pts',(1.70119600494326,-2.40603518007504,2.67012712010573));
#18346=CARTESIAN_POINT('Ctrl Pts',(0.91051086378161,-2.965092006437,2.61750674973535));
#18347=CARTESIAN_POINT('Ctrl Pts',(-0.182644352078765,-3.09635938647313,
2.56488637936498));
#18348=CARTESIAN_POINT('Ctrl Pts',(-1.08320700768761,-2.74038967310636,
2.51226600899461));
#18349=CARTESIAN_POINT('Ctrl Pts',(-1.98376966329644,-2.3844199597396,2.45964563862424));
#18350=CARTESIAN_POINT('Ctrl Pts',(-2.69173975865374,-1.54121315296996,
2.40702526825387));
#18351=CARTESIAN_POINT('Ctrl Pts',(-2.88649532799773,-0.59263639450121,
2.3544048978835));
#18352=CARTESIAN_POINT('Ctrl Pts',(-2.92625644781122,-0.398975826678611,
2.3436619709522));
#18353=CARTESIAN_POINT('Ctrl Pts',(-2.94462630681883,-0.200923340849699,
2.3329190440209));
#18354=CARTESIAN_POINT('Ctrl Pts',(-2.94283216929169,-0.00254059509496668,
2.3221761170896));
#18355=CARTESIAN_POINT('Ctrl Pts',(-2.94249560619114,-0.00258942729680482,
2.17782388291039));
#18356=CARTESIAN_POINT('Ctrl Pts',(-2.94440414260591,-0.212580342560449,
2.18919207994051));
#18357=CARTESIAN_POINT('Ctrl Pts',(-2.92381470891138,-0.422199995772688,
2.20056027697063));
#18358=CARTESIAN_POINT('Ctrl Pts',(-2.87932772554241,-0.626618874207943,
2.21192847400075));
#18359=CARTESIAN_POINT('Ctrl Pts',(-2.67323476668884,-1.57362153232989,
2.26459343766743));
#18360=CARTESIAN_POINT('Ctrl Pts',(-1.95426416634525,-2.40900768006153,
2.31725840133412));
#18361=CARTESIAN_POINT('Ctrl Pts',(-1.04852602468143,-2.75386472764491,
2.3699233650008));
#18362=CARTESIAN_POINT('Ctrl Pts',(-0.142787883017607,-3.09872177522829,
2.42258832866749));
#18363=CARTESIAN_POINT('Ctrl Pts',(0.949717799966449,-2.95304972266342,
2.47525329233417));
#18364=CARTESIAN_POINT('Ctrl Pts',(1.7334537997702,-2.38292188563198,2.52791825600086));
#18365=CARTESIAN_POINT('Ctrl Pts',(2.51718979957395,-1.81279404860055,2.58058321966754));
#18366=CARTESIAN_POINT('Ctrl Pts',(2.99215611619739,-0.818210427102559,
2.63324818333423));
#18367=CARTESIAN_POINT('Ctrl Pts',(2.94291803037279,0.149706737509724,2.68591314700091));
#18368=CARTESIAN_POINT('Ctrl Pts',(2.89367994454819,1.11762390212201,2.7385781106676));
#18369=CARTESIAN_POINT('Ctrl Pts',(2.32023745627556,2.05887460984858,2.79124307433428));
#18370=CARTESIAN_POINT('Ctrl Pts',(1.4826919461771,2.54652764310569,2.84390803800096));
#18371=CARTESIAN_POINT('Ctrl Pts',(0.645146436078633,3.03418067636279,2.89657300166765));
#18372=CARTESIAN_POINT('Ctrl Pts',(-0.456502095845658,3.06823603515044,
2.94923796533433));
#18373=CARTESIAN_POINT('Ctrl Pts',(-1.32256928803916,2.63324686948073,3.00190292900102));
#18374=CARTESIAN_POINT('Ctrl Pts',(-2.18863648023266,2.19825770381101,3.0545678926677));
#18375=CARTESIAN_POINT('Ctrl Pts',(-2.81912233269536,1.29422401368392,3.10723285633439));
#18376=CARTESIAN_POINT('Ctrl Pts',(-2.92805183726137,0.331196319314338,
3.15989782000107));
#18377=CARTESIAN_POINT('Ctrl Pts',(-2.94041095304778,0.221931425219236,
3.16587317430418));
#18378=CARTESIAN_POINT('Ctrl Pts',(-2.94605601250203,0.111907094355046,
3.17184852860728));
#18379=CARTESIAN_POINT('Ctrl Pts',(-2.94526037616607,0.00180040430511289,
3.17782388291039));
#18380=CARTESIAN_POINT('Origin',(0.,0.,0.));
#18381=CARTESIAN_POINT('',(-2.93739242931988,0.000540407572186541,4.3221761170896));
#18382=CARTESIAN_POINT('',(-2.93753500859377,0.000882026442511373,4.17782388291039));
#18383=CARTESIAN_POINT('',(-2.942,-3.60291088309151E-16,0.));
#18384=CARTESIAN_POINT('Ctrl Pts',(-2.93739242931988,0.000540407572186541,
4.3221761170896));
#18385=CARTESIAN_POINT('Ctrl Pts',(-2.93814630501522,0.454709257120266,
4.29769682179868));
#18386=CARTESIAN_POINT('Ctrl Pts',(-2.83910536028106,0.908566671316128,
4.27321752650776));
#18387=CARTESIAN_POINT('Ctrl Pts',(-2.6385374625564,1.31194251096478,4.24873823121684));
#18388=CARTESIAN_POINT('Ctrl Pts',(-2.20739935432037,2.17903389691023,4.19611786084646));
#18389=CARTESIAN_POINT('Ctrl Pts',(-1.30713327152341,2.8128638865229,4.14349749047609));
#18390=CARTESIAN_POINT('Ctrl Pts',(-0.345447198709921,2.92638673563265,
4.09087712010572));
#18391=CARTESIAN_POINT('Ctrl Pts',(0.616238874103564,3.0399095847424,4.03825674973536));
#18392=CARTESIAN_POINT('Ctrl Pts',(1.63934493693357,2.63312529334921,3.98563637936499));
#18393=CARTESIAN_POINT('Ctrl Pts',(2.26053185174972,1.89025628960273,3.93301600899462));
#18394=CARTESIAN_POINT('Ctrl Pts',(2.88171876656588,1.14738728585625,3.88039563862425));
#18395=CARTESIAN_POINT('Ctrl Pts',(3.10098653336818,0.0684335697564567,
3.82777526825387));
#18396=CARTESIAN_POINT('Ctrl Pts',(2.8190342665149,-0.857973716122647,3.7751548978835));
#18397=CARTESIAN_POINT('Ctrl Pts',(2.53708199966161,-1.78438100200175,3.72253452751313));
#18398=CARTESIAN_POINT('Ctrl Pts',(1.75390969915275,-2.55824185766015,3.66991415714276));
#18399=CARTESIAN_POINT('Ctrl Pts',(0.824196505293748,-2.82909406262337,
3.61729378677239));
#18400=CARTESIAN_POINT('Ctrl Pts',(-0.105516688565254,-3.09994626758658,
3.56467341640202));
#18401=CARTESIAN_POINT('Ctrl Pts',(-1.18177077577439,-2.86778982185459,
3.51205304603165));
#18402=CARTESIAN_POINT('Ctrl Pts',(-1.91715720801869,-2.23776257255722,
3.45943267566128));
#18403=CARTESIAN_POINT('Ctrl Pts',(-2.55655857926025,-1.68996855643583,
3.41368048947072));
#18404=CARTESIAN_POINT('Ctrl Pts',(-2.93826750108625,-0.841388295482023,
3.36792830328016));
#18405=CARTESIAN_POINT('Ctrl Pts',(-2.94484294150901,0.00199174253909633,
3.3221761170896));
#18406=CARTESIAN_POINT('Ctrl Pts',(-2.94526037616607,0.00180040430511289,
3.17782388291039));
#18407=CARTESIAN_POINT('Ctrl Pts',(-2.93904351473207,-0.858539934689441,
3.22451349227397));
#18408=CARTESIAN_POINT('Ctrl Pts',(-2.53959728591596,-1.72390862024193,
3.27120310163755));
#18409=CARTESIAN_POINT('Ctrl Pts',(-1.87733008879233,-2.27130145042432,
3.31789271100113));
#18410=CARTESIAN_POINT('Ctrl Pts',(-1.13030567908798,-2.88874982718133,
3.37055767466781));
#18411=CARTESIAN_POINT('Ctrl Pts',(-0.0488837030099704,-3.10162488208327,
3.4232226383345));
#18412=CARTESIAN_POINT('Ctrl Pts',(0.876425794829888,-2.81337100100799,
3.47588760200118));
#18413=CARTESIAN_POINT('Ctrl Pts',(1.80173529266975,-2.5251171199327,3.52855256566786));
#18414=CARTESIAN_POINT('Ctrl Pts',(2.57093231227146,-1.73573430288019,3.58121752933455));
#18415=CARTESIAN_POINT('Ctrl Pts',(2.83512541526138,-0.803269840348294,
3.63388249300123));
#18416=CARTESIAN_POINT('Ctrl Pts',(3.0993185182513,0.129194622183599,3.68654745666792));
#18417=CARTESIAN_POINT('Ctrl Pts',(2.85850770462944,1.20474073019488,3.7392124203346));
#18418=CARTESIAN_POINT('Ctrl Pts',(2.22191964750238,1.93552360728328,3.79187738400129));
#18419=CARTESIAN_POINT('Ctrl Pts',(1.58533159037532,2.66630648437168,3.84454234766797));
#18420=CARTESIAN_POINT('Ctrl Pts',(0.552966289743035,3.05232613053722,3.89720731133465));
#18421=CARTESIAN_POINT('Ctrl Pts',(-0.406917273431679,2.91849222887777,
3.94987227500134));
#18422=CARTESIAN_POINT('Ctrl Pts',(-1.36680083660641,2.78465832721833,4.00253723866802));
#18423=CARTESIAN_POINT('Ctrl Pts',(-2.25420266232356,2.13097087773392,4.05520220233471));
#18424=CARTESIAN_POINT('Ctrl Pts',(-2.666616123304,1.25392862924115,4.10786716600139));
#18425=CARTESIAN_POINT('Ctrl Pts',(-2.84922387445754,0.865593310885713,
4.13118607163773));
#18426=CARTESIAN_POINT('Ctrl Pts',(-2.9387088904313,0.433468688742346,4.15450497727406));
#18427=CARTESIAN_POINT('Ctrl Pts',(-2.93753500859377,0.000882026442511374,
4.17782388291039));
#18428=CARTESIAN_POINT('Origin',(0.,0.,0.));
#18429=CARTESIAN_POINT('',(-2.94294893056736,-0.00252441656932667,5.3221761170896));
#18430=CARTESIAN_POINT('',(-2.94214529852914,-0.00261326515612426,5.1778238829104));
#18431=CARTESIAN_POINT('',(-2.942,-3.60291088309151E-16,0.));
#18432=CARTESIAN_POINT('Ctrl Pts',(-2.94294893056736,-0.00252441656932667,
5.3221761170896));
#18433=CARTESIAN_POINT('Ctrl Pts',(-2.93593381851913,0.774652637504292,
5.28008571068756));
#18434=CARTESIAN_POINT('Ctrl Pts',(-2.61899610205614,1.55689120032164,5.23799530428553));
#18435=CARTESIAN_POINT('Ctrl Pts',(-2.06692649506365,2.10021140779169,5.1959048978835));
#18436=CARTESIAN_POINT('Ctrl Pts',(-1.37674291943613,2.77945670358908,5.14328452751313));
#18437=CARTESIAN_POINT('Ctrl Pts',(-0.31906293568821,3.08528758407071,5.09066415714276));
#18438=CARTESIAN_POINT('Ctrl Pts',(0.627116654359043,2.8792008952563,5.03804378677239));
#18439=CARTESIAN_POINT('Ctrl Pts',(1.5732962444063,2.67311420644189,4.98542341640202));
#18440=CARTESIAN_POINT('Ctrl Pts',(2.4079754407529,1.95510994833143,4.93280304603165));
#18441=CARTESIAN_POINT('Ctrl Pts',(2.75314891878373,1.05035428518759,4.88018267566128));
#18442=CARTESIAN_POINT('Ctrl Pts',(3.09832239681456,0.145598622043775,4.82756230529091));
#18443=CARTESIAN_POINT('Ctrl Pts',(2.95399015652965,-0.945908446133409,
4.77494193492054));
#18444=CARTESIAN_POINT('Ctrl Pts',(2.38551665840565,-1.72985067733577,4.72232156455017));
#18445=CARTESIAN_POINT('Ctrl Pts',(1.81704316028163,-2.51379290853814,4.6697011941798));
#18446=CARTESIAN_POINT('Ctrl Pts',(0.824428404318513,-2.99017030276568,
4.61708082380943));
#18447=CARTESIAN_POINT('Ctrl Pts',(-0.142797221412707,-2.9432434569701,
4.56446045343906));
#18448=CARTESIAN_POINT('Ctrl Pts',(-1.11002284714393,-2.89631661117452,
4.51184008306869));
#18449=CARTESIAN_POINT('Ctrl Pts',(-2.05185934264326,-2.32608552535581,
4.45921971269832));
#18450=CARTESIAN_POINT('Ctrl Pts',(-2.54177252355539,-1.49079359130735,
4.40659934232795));
#18451=CARTESIAN_POINT('Ctrl Pts',(-2.80377530896762,-1.04408421119714,
4.3784582672485));
#18452=CARTESIAN_POINT('Ctrl Pts',(-2.93652578376122,-0.52156611314212,
4.35031719216905));
#18453=CARTESIAN_POINT('Ctrl Pts',(-2.93739242931988,0.000540407572186541,
4.3221761170896));
#18454=CARTESIAN_POINT('Ctrl Pts',(-2.93753500859377,0.000882026442511374,
4.17782388291039));
#18455=CARTESIAN_POINT('Ctrl Pts',(-2.93605771780397,-0.543513730930775,
4.20716994094074));
#18456=CARTESIAN_POINT('Ctrl Pts',(-2.79100052624987,-1.08864123864977,
4.23651599897109));
#18457=CARTESIAN_POINT('Ctrl Pts',(-2.50727405993036,-1.54814577624058,
4.26586205700145));
#18458=CARTESIAN_POINT('Ctrl Pts',(-1.99809343933257,-2.37278088572845,
4.31852702066813));
#18459=CARTESIAN_POINT('Ctrl Pts',(-1.04230710189327,-2.92165405720309,
4.37119198433482));
#18460=CARTESIAN_POINT('Ctrl Pts',(-0.0734394371752462,-2.94580807344744,
4.4238569480015));
#18461=CARTESIAN_POINT('Ctrl Pts',(0.895428227542791,-2.9699620896918,4.47652191166818));
#18462=CARTESIAN_POINT('Ctrl Pts',(1.87737721953956,-2.46939695070584,4.52918687533487));
#18463=CARTESIAN_POINT('Ctrl Pts',(2.427016324523,-1.67115837574717,4.58185183900155));
#18464=CARTESIAN_POINT('Ctrl Pts',(2.97665542950643,-0.872919800788501,
4.63451680266824));
#18465=CARTESIAN_POINT('Ctrl Pts',(3.09398464747655,0.22299221014288,4.68718176633492));
#18466=CARTESIAN_POINT('Ctrl Pts',(2.725785936287,1.11949523708763,4.73984673000161));
#18467=CARTESIAN_POINT('Ctrl Pts',(2.35758722509745,2.01599826403239,4.79251169366829));
#18468=CARTESIAN_POINT('Ctrl Pts',(1.50386058474821,2.71309230699052,4.84517665733498));
#18469=CARTESIAN_POINT('Ctrl Pts',(0.551838293166775,2.8945903085884,4.89784162100166));
#18470=CARTESIAN_POINT('Ctrl Pts',(-0.400183998414646,3.07608831018627,
4.95050658466835));
#18471=CARTESIAN_POINT('Ctrl Pts',(-1.45050194122825,2.74199027042391,5.00317154833503));
#18472=CARTESIAN_POINT('Ctrl Pts',(-2.12271361651498,2.04383596665945,5.05583651200172));
#18473=CARTESIAN_POINT('Ctrl Pts',(-2.64172618991724,1.50479316935294,5.09649896897128));
#18474=CARTESIAN_POINT('Ctrl Pts',(-2.93533688440644,0.748724173372516,
5.13716142594084));
#18475=CARTESIAN_POINT('Ctrl Pts',(-2.94214529852914,-0.00261326515612426,
5.1778238829104));
#18476=CARTESIAN_POINT('Origin',(0.,0.,0.));
#18477=CARTESIAN_POINT('',(-2.94474230559933,0.0020353165097306,6.3221761170896));
#18478=CARTESIAN_POINT('',(-2.94552589459255,0.00164462538419303,6.1778238829104));
#18479=CARTESIAN_POINT('',(-2.942,-3.60291088309151E-16,0.));
#18480=CARTESIAN_POINT('Ctrl Pts',(-2.94474230559933,0.0020353165097306,
6.3221761170896));
#18481=CARTESIAN_POINT('Ctrl Pts',(-2.94577608567865,0.132578411608025,
6.31509496994683));
#18482=CARTESIAN_POINT('Ctrl Pts',(-2.93783733482844,0.262995037552802,
6.30801382280405));
#18483=CARTESIAN_POINT('Ctrl Pts',(-2.92049520368276,0.39214902611321,6.30093267566128));
#18484=CARTESIAN_POINT('Ctrl Pts',(-2.79162493090094,1.35189898976081,6.24831230529091));
#18485=CARTESIAN_POINT('Ctrl Pts',(-2.1434950231737,2.24192544902223,6.19569193492054));
#18486=CARTESIAN_POINT('Ctrl Pts',(-1.26962729970534,2.65915768867859,6.14307156455017));
#18487=CARTESIAN_POINT('Ctrl Pts',(-0.395759576236975,3.07638992833495,
6.0904511941798));
#18488=CARTESIAN_POINT('Ctrl Pts',(0.70384596297251,3.02082794838624,6.03783082380943));
#18489=CARTESIAN_POINT('Ctrl Pts',(1.53120548099802,2.51763437940803,5.98521045343906));
#18490=CARTESIAN_POINT('Ctrl Pts',(2.35856499902354,2.0144408104298,5.93259008306869));
#18491=CARTESIAN_POINT('Ctrl Pts',(2.91367849586509,1.06361565242206,5.87996971269832));
#18492=CARTESIAN_POINT('Ctrl Pts',(2.9451489575673,0.0957638301017936,5.82734934232795));
#18493=CARTESIAN_POINT('Ctrl Pts',(2.97661941926951,-0.872087992218468,
5.77472897195758));
#18494=CARTESIAN_POINT('Ctrl Pts',(2.48444684583239,-1.85696647885126,5.72210860158721));
#18495=CARTESIAN_POINT('Ctrl Pts',(1.69152388176343,-2.41284480454905,5.66948823121684));
#18496=CARTESIAN_POINT('Ctrl Pts',(0.898600917694462,-2.96872313024685,
5.61686786084646));
#18497=CARTESIAN_POINT('Ctrl Pts',(-0.19507243700635,-3.09560129500965,
5.56424749047609));
#18498=CARTESIAN_POINT('Ctrl Pts',(-1.09419888335647,-2.73601935246765,
5.51162712010572));
#18499=CARTESIAN_POINT('Ctrl Pts',(-1.9933253297066,-2.37643740992565,5.45900674973535));
#18500=CARTESIAN_POINT('Ctrl Pts',(-2.69790486770603,-1.53039536007885,
5.40638637936499));
#18501=CARTESIAN_POINT('Ctrl Pts',(-2.88885105295217,-0.581044479598858,
5.35376600899461));
#18502=CARTESIAN_POINT('Ctrl Pts',(-2.92706166295704,-0.391068040923041,
5.34323604502627));
#18503=CARTESIAN_POINT('Ctrl Pts',(-2.94470393564848,-0.196954622309047,
5.33270608105794));
#18504=CARTESIAN_POINT('Ctrl Pts',(-2.94294893056736,-0.00252441656932667,
5.3221761170896));
#18505=CARTESIAN_POINT('Ctrl Pts',(-2.94214529852914,-0.00261326515612426,
5.1778238829104));
#18506=CARTESIAN_POINT('Ctrl Pts',(-2.94415496646843,-0.224388664623296,
5.18982638960752));
#18507=CARTESIAN_POINT('Ctrl Pts',(-2.92117618657372,-0.445751813963285,
5.20182889630465));
#18508=CARTESIAN_POINT('Ctrl Pts',(-2.87162987121487,-0.660999575716158,
5.21383140300177));
#18509=CARTESIAN_POINT('Ctrl Pts',(-2.65422904286817,-1.60547024656074,
5.26649636666845));
#18510=CARTESIAN_POINT('Ctrl Pts',(-1.92532197841492,-2.43220102048334,
5.31916133033513));
#18511=CARTESIAN_POINT('Ctrl Pts',(-1.01552544630456,-2.76620437138433,
5.37182629400182));
#18512=CARTESIAN_POINT('Ctrl Pts',(-0.105728914194198,-3.10020772228531,
5.4244912576685));
#18513=CARTESIAN_POINT('Ctrl Pts',(0.984957085573281,-2.94148365016469,
5.47715622133519));
#18514=CARTESIAN_POINT('Ctrl Pts',(1.761820540694,-2.36202602414577,5.52982118500188));
#18515=CARTESIAN_POINT('Ctrl Pts',(2.53868399581473,-1.78256839812686,5.58248614866856));
#18516=CARTESIAN_POINT('Ctrl Pts',(3.0017249062887,-0.782377218209647,5.63515111233524));
#18517=CARTESIAN_POINT('Ctrl Pts',(2.94091774630216,0.184882032222853,5.68781607600193));
#18518=CARTESIAN_POINT('Ctrl Pts',(2.88011058631563,1.15214128265535,5.74048103966861));
#18519=CARTESIAN_POINT('Ctrl Pts',(2.2954553558686,2.08646860360313,5.7931460033353));
#18520=CARTESIAN_POINT('Ctrl Pts',(1.45213925422783,2.56407295970403,5.84581096700198));
#18521=CARTESIAN_POINT('Ctrl Pts',(0.60882315258705,3.04167731580494,5.89847593066867));
#18522=CARTESIAN_POINT('Ctrl Pts',(-0.493153820247473,3.06255870705896,
5.95114089433535));
#18523=CARTESIAN_POINT('Ctrl Pts',(-1.35395830631657,2.6172457777424,6.00380585800203));
#18524=CARTESIAN_POINT('Ctrl Pts',(-2.21476279238567,2.17193284842583,6.05647082166872));
#18525=CARTESIAN_POINT('Ctrl Pts',(-2.83439479168936,1.26042559853868,6.10913578533541));
#18526=CARTESIAN_POINT('Ctrl Pts',(-2.93180238522596,0.296164363719765,
6.16180074900209));
#18527=CARTESIAN_POINT('Ctrl Pts',(-2.94168102690256,0.198373309905978,
6.1671417936382));
#18528=CARTESIAN_POINT('Ctrl Pts',(-2.94618853440423,0.100039675683843,
6.1724828382743));
#18529=CARTESIAN_POINT('Ctrl Pts',(-2.94552589459255,0.00164462538419303,
6.1778238829104));
#18530=CARTESIAN_POINT('Origin',(0.,0.,0.));
#18531=CARTESIAN_POINT('',(-2.93737184280031,0.000478285809368539,7.32217611708959));
#18532=CARTESIAN_POINT('',(-2.93765213932985,0.00105817779144944,7.17782388291039));
#18533=CARTESIAN_POINT('',(-2.942,-3.60291088309151E-16,0.));
#18534=CARTESIAN_POINT('Ctrl Pts',(-2.93737184280031,0.000478285809368539,
7.32217611708959));
#18535=CARTESIAN_POINT('Ctrl Pts',(-2.93804459091945,0.458606303769958,
7.29748385883571));
#18536=CARTESIAN_POINT('Ctrl Pts',(-2.83719423177179,0.916453996322869,
7.27279160058183));
#18537=CARTESIAN_POINT('Ctrl Pts',(-2.63324974290992,1.32252368027208,7.24809934232795));
#18538=CARTESIAN_POINT('Ctrl Pts',(-2.198634389848,2.18787738530332,7.19547897195758));
#18539=CARTESIAN_POINT('Ctrl Pts',(-1.29583121079705,2.81808837804428,7.14285860158721));
#18540=CARTESIAN_POINT('Ctrl Pts',(-0.333697177699206,2.92774986756231,
7.09023823121684));
#18541=CARTESIAN_POINT('Ctrl Pts',(0.628436855398639,3.03741135708034,7.03761786084647));
#18542=CARTESIAN_POINT('Ctrl Pts',(1.64990174254338,2.62652334337548,6.9849974904761));
#18543=CARTESIAN_POINT('Ctrl Pts',(2.26810159307568,1.88116672756646,6.93237712010573));
#18544=CARTESIAN_POINT('Ctrl Pts',(2.886301443608,1.13581011175742,6.87975674973536));
#18545=CARTESIAN_POINT('Ctrl Pts',(3.10123625752784,0.055984893844227,6.82713637936498));
#18546=CARTESIAN_POINT('Ctrl Pts',(2.81556743521199,-0.869283101865742,
6.77451600899461));
#18547=CARTESIAN_POINT('Ctrl Pts',(2.52989861289615,-1.7945510975757,6.72189563862424));
#18548=CARTESIAN_POINT('Ctrl Pts',(1.74362615434463,-2.56526187108243,6.66927526825387));
#18549=CARTESIAN_POINT('Ctrl Pts',(0.812833183747132,-2.8323797960046,6.6166548978835));
#18550=CARTESIAN_POINT('Ctrl Pts',(-0.117959786850361,-3.09949772092676,
6.56403452751313));
#18551=CARTESIAN_POINT('Ctrl Pts',(-1.19327326949384,-2.86302279726437,
6.51141415714276));
#18552=CARTESIAN_POINT('Ctrl Pts',(-1.92612469189739,-2.23004860141629,
6.45879378677239));
#18553=CARTESIAN_POINT('Ctrl Pts',(-2.56035596550109,-1.68225403062272,
6.41325456354479));
#18554=CARTESIAN_POINT('Ctrl Pts',(-2.93809401248361,-0.83749407451141,
6.3677153403172));
#18555=CARTESIAN_POINT('Ctrl Pts',(-2.94474230559933,0.0020353165097306,
6.3221761170896));
#18556=CARTESIAN_POINT('Ctrl Pts',(-2.94552589459255,0.00164462538419303,
6.1778238829104));
#18557=CARTESIAN_POINT('Ctrl Pts',(-2.93965462503178,-0.87017722046166,
6.22514780194098));
#18558=CARTESIAN_POINT('Ctrl Pts',(-2.52789003171806,-1.74682066505967,
6.27247172097156));
#18559=CARTESIAN_POINT('Ctrl Pts',(-1.85003983495055,-2.2935847848838,6.31979564000214));
#18560=CARTESIAN_POINT('Ctrl Pts',(-1.095686503369,-2.90205747891776,6.37246060366883));
#18561=CARTESIAN_POINT('Ctrl Pts',(-0.0117966524363787,-3.10198764723502,
6.42512556733551));
#18562=CARTESIAN_POINT('Ctrl Pts',(0.910000294361383,-2.80269121035772,
6.4777905310022));
#18563=CARTESIAN_POINT('Ctrl Pts',(1.83179724115916,-2.50339477348041,6.53045549466888));
#18564=CARTESIAN_POINT('Ctrl Pts',(2.59150128382206,-1.70487173140855,6.58312045833556));
#18565=CARTESIAN_POINT('Ctrl Pts',(2.8445267984577,-0.769315181970455,6.63578542200225));
#18566=CARTESIAN_POINT('Ctrl Pts',(3.09755231309333,0.166241367467632,6.68845038566893));
#18567=CARTESIAN_POINT('Ctrl Pts',(2.84389929970168,1.23883142427194,6.74111534933562));
#18568=CARTESIAN_POINT('Ctrl Pts',(2.19861937965545,1.96195091165853,6.79378031300231));
#18569=CARTESIAN_POINT('Ctrl Pts',(1.55333945960922,2.68507039904512,6.84644527666899));
#18570=CARTESIAN_POINT('Ctrl Pts',(0.51643263290838,3.05871931701401,6.89911024033567));
#18571=CARTESIAN_POINT('Ctrl Pts',(-0.441782179220013,2.91341844960141,
6.95177520400236));
#18572=CARTESIAN_POINT('Ctrl Pts',(-1.39999699134843,2.76811758218879,7.00444016766904));
#18573=CARTESIAN_POINT('Ctrl Pts',(-2.2795197889044,2.10386692939468,7.05710513133573));
#18574=CARTESIAN_POINT('Ctrl Pts',(-2.68141770473996,1.22195648411116,7.10977009500241));
#18575=CARTESIAN_POINT('Ctrl Pts',(-2.85452884366231,0.842087578115104,
7.13245469097174));
#18576=CARTESIAN_POINT('Ctrl Pts',(-2.93902534565796,0.421835844039577,
7.15513928694107));
#18577=CARTESIAN_POINT('Ctrl Pts',(-2.93765213932985,0.00105817779144944,
7.17782388291039));
#18578=CARTESIAN_POINT('Origin',(0.,0.,0.));
#18579=CARTESIAN_POINT('',(-2.94306537549688,-0.00250657139928612,8.3221761170896));
#18580=CARTESIAN_POINT('',(-2.94179645842688,-0.00262223567938445,8.17782388291039));
#18581=CARTESIAN_POINT('',(-2.942,-3.60291088309151E-16,0.));
#18582=CARTESIAN_POINT('Ctrl Pts',(-2.94306537549688,-0.00250657139928612,
8.3221761170896));
#18583=CARTESIAN_POINT('Ctrl Pts',(-2.93603346312234,0.778523040326291,
8.2798727477246));
#18584=CARTESIAN_POINT('Ctrl Pts',(-2.6155295502631,1.5646541741046,8.23756937835961));
#18585=CARTESIAN_POINT('Ctrl Pts',(-2.0584790752992,2.10849163858216,8.19526600899462));
#18586=CARTESIAN_POINT('Ctrl Pts',(-1.36557440251332,2.78496089461673,8.14264563862425));
#18587=CARTESIAN_POINT('Ctrl Pts',(-0.306675260078988,3.08654352280986,
8.09002526825387));
#18588=CARTESIAN_POINT('Ctrl Pts',(0.638669423716989,2.87666029635488,8.0374048978835));
#18589=CARTESIAN_POINT('Ctrl Pts',(1.58401410751295,2.66677706989991,7.98478452751313));
#18590=CARTESIAN_POINT('Ctrl Pts',(2.41580433267058,1.94542798879682,7.93216415714276));
#18591=CARTESIAN_POINT('Ctrl Pts',(2.75734311734437,1.03929400395132,7.87954378677239));
#18592=CARTESIAN_POINT('Ctrl Pts',(3.09888190201817,0.133160019105817,7.82692341640202));
#18593=CARTESIAN_POINT('Ctrl Pts',(2.95016924620815,-0.957758869482093,
7.77430304603165));
#18594=CARTESIAN_POINT('Ctrl Pts',(2.37855339098706,-1.73941279161662,7.72168267566128));
#18595=CARTESIAN_POINT('Ctrl Pts',(1.80693753576595,-2.52106671375116,7.66906230529091));
#18596=CARTESIAN_POINT('Ctrl Pts',(0.812418481133763,-2.99345566943229,
7.61644193492054));
#18597=CARTESIAN_POINT('Ctrl Pts',(-0.154610975618871,-2.94264651965433,
7.56382156455017));
#18598=CARTESIAN_POINT('Ctrl Pts',(-1.1216404323715,-2.89183736987637,7.5112011941798));
#18599=CARTESIAN_POINT('Ctrl Pts',(-2.06118029124457,-2.31783011463932,
7.45858082380943));
#18600=CARTESIAN_POINT('Ctrl Pts',(-2.54773645714466,-1.48057827836003,
7.40596045343906));
#18601=CARTESIAN_POINT('Ctrl Pts',(-2.80597476023112,-1.03620924430037,
7.37803234132257));
#18602=CARTESIAN_POINT('Ctrl Pts',(-2.93661093285418,-0.517686173583286,
7.35010422920608));
#18603=CARTESIAN_POINT('Ctrl Pts',(-2.93737184280031,0.000478285809368539,
7.32217611708959));
#18604=CARTESIAN_POINT('Ctrl Pts',(-2.93765213932985,0.00105817779144944,
7.17782388291039));
#18605=CARTESIAN_POINT('Ctrl Pts',(-2.93583728528984,-0.555049110608679,
7.20780425060775));
#18606=CARTESIAN_POINT('Ctrl Pts',(-2.78403605908896,-1.11207503097007,
7.23778461830511));
#18607=CARTESIAN_POINT('Ctrl Pts',(-2.48858495099342,-1.57801251517323,
7.26776498600247));
#18608=CARTESIAN_POINT('Ctrl Pts',(-1.96958124729618,-2.39650083140119,
7.32042994966915));
#18609=CARTESIAN_POINT('Ctrl Pts',(-1.00730080578659,-2.93390722608419,
7.37309491333584));
#18610=CARTESIAN_POINT('Ctrl Pts',(-0.0382136038189444,-2.94647556868157,
7.42575987700252));
#18611=CARTESIAN_POINT('Ctrl Pts',(0.930873598148709,-2.95904391127895,
7.47842484066921));
#18612=CARTESIAN_POINT('Ctrl Pts',(1.90676756057442,-2.44677420179069,7.53108980433588));
#18613=CARTESIAN_POINT('Ctrl Pts',(2.44682350205541,-1.64202110404938,7.58375476800257));
#18614=CARTESIAN_POINT('Ctrl Pts',(2.98687944353639,-0.837268006308086,
7.63641973166925));
#18615=CARTESIAN_POINT('Ctrl Pts',(3.09109736407267,0.25996847968624,7.68908469533594));
#18616=CARTESIAN_POINT('Ctrl Pts',(2.71220622763963,1.15200518015635,7.74174965900263));
#18617=CARTESIAN_POINT('Ctrl Pts',(2.33331509120659,2.04404188062646,7.79441462266931));
#18618=CARTESIAN_POINT('Ctrl Pts',(1.47131489780423,2.73087879557235,7.84707958633599));
#18619=CARTESIAN_POINT('Ctrl Pts',(0.517190633372317,2.90098128313613,7.89974455000268));
#18620=CARTESIAN_POINT('Ctrl Pts',(-0.436933631059594,3.07108377069992,
7.95240951366936));
#18621=CARTESIAN_POINT('Ctrl Pts',(-1.48318196652107,2.72445183088159,8.00507447733605));
#18622=CARTESIAN_POINT('Ctrl Pts',(-2.14699834174799,2.01831035197405,8.05773944100273));
#18623=CARTESIAN_POINT('Ctrl Pts',(-2.65153376339188,1.48160562142403,8.09776758830529));
#18624=CARTESIAN_POINT('Ctrl Pts',(-2.93514585523751,0.737219387421443,
8.13779573560784));
#18625=CARTESIAN_POINT('Ctrl Pts',(-2.94179645842688,-0.00262223567938445,
8.17782388291039));
#18626=CARTESIAN_POINT('Origin',(0.,0.,0.));
#18627=CARTESIAN_POINT('',(-2.94464008512449,0.00207742171232136,9.3221761170896));
#18628=CARTESIAN_POINT('',(-2.94577110767244,0.00147777103002609,9.1778238829104));
#18629=CARTESIAN_POINT('',(-2.942,-3.60291088309151E-16,0.));
#18630=CARTESIAN_POINT('Ctrl Pts',(-2.94464008512449,0.00207742171232136,
9.3221761170896));
#18631=CARTESIAN_POINT('Ctrl Pts',(-2.94572064417758,0.136558752036829,
9.31488200698387));
#18632=CARTESIAN_POINT('Ctrl Pts',(-2.93729508396668,0.270903986837675,
9.30758789687813));
#18633=CARTESIAN_POINT('Ctrl Pts',(-2.91889749004766,0.4038694541666,9.3002937867724));
#18634=CARTESIAN_POINT('Ctrl Pts',(-2.7861755826581,1.3630943679524,9.24767341640203));
#18635=CARTESIAN_POINT('Ctrl Pts',(-2.1344781113937,2.25051190295123,9.19505304603165));
#18636=CARTESIAN_POINT('Ctrl Pts',(-1.25894255572533,2.66423286046833,9.14243267566128));
#18637=CARTESIAN_POINT('Ctrl Pts',(-0.383407000056953,3.07795381798544,
9.08981230529091));
#18638=CARTESIAN_POINT('Ctrl Pts',(0.715966640015389,3.01797819802083,9.03719193492054));
#18639=CARTESIAN_POINT('Ctrl Pts',(1.54129954888374,2.51146745828537,8.98457156455017));
#18640=CARTESIAN_POINT('Ctrl Pts',(2.3666324577521,2.00495671854991,8.9319511941798));
#18641=CARTESIAN_POINT('Ctrl Pts',(2.91792463541645,1.05191085904358,8.87933082380943));
#18642=CARTESIAN_POINT('Ctrl Pts',(2.94550964776859,0.0839405046308018,
8.82671045343906));
#18643=CARTESIAN_POINT('Ctrl Pts',(2.97309466012074,-0.884029849781979,
8.77409008306869));
#18644=CARTESIAN_POINT('Ctrl Pts',(2.47697250716068,-1.86692469910122,8.72146971269832));
#18645=CARTESIAN_POINT('Ctrl Pts',(1.68182449914462,-2.41961555778857,8.66884934232795));
#18646=CARTESIAN_POINT('Ctrl Pts',(0.886676491128584,-2.97230641647591,
8.61622897195757));
#18647=CARTESIAN_POINT('Ctrl Pts',(-0.207497371943416,-3.09479328453138,
8.56360860158721));
#18648=CARTESIAN_POINT('Ctrl Pts',(-1.10517312337017,-2.73160492399537,
8.51098823121684));
#18649=CARTESIAN_POINT('Ctrl Pts',(-2.00284887479693,-2.36841656345936,
8.45836786084647));
#18650=CARTESIAN_POINT('Ctrl Pts',(-2.70402651457844,-1.51955297433185,
8.4057474904761));
#18651=CARTESIAN_POINT('Ctrl Pts',(-2.89116023290047,-0.56944323783011,
8.35312712010573));
#18652=CARTESIAN_POINT('Ctrl Pts',(-2.92785056302318,-0.383160187412328,
8.34281011910035));
#18653=CARTESIAN_POINT('Ctrl Pts',(-2.94478032747652,-0.192985093804385,
8.33249311809497));
#18654=CARTESIAN_POINT('Ctrl Pts',(-2.94306537549688,-0.00250657139928612,
8.3221761170896));
#18655=CARTESIAN_POINT('Ctrl Pts',(-2.94179645842688,-0.00262223567938445,
8.17782388291039));
#18656=CARTESIAN_POINT('Ctrl Pts',(-2.94389604226671,-0.236188947098698,
8.19046069927452));
#18657=CARTESIAN_POINT('Ctrl Pts',(-2.91839215134056,-0.469302718100354,
8.20309751563865));
#18658=CARTESIAN_POINT('Ctrl Pts',(-2.86352159037298,-0.695286025907358,
8.21573433200279));
#18659=CARTESIAN_POINT('Ctrl Pts',(-2.63484404877868,-1.63708990688444,
8.26839929566947));
#18660=CARTESIAN_POINT('Ctrl Pts',(-1.89610455059774,-2.45504665084187,
8.32106425933616));
#18661=CARTESIAN_POINT('Ctrl Pts',(-0.982379647459882,-2.77814844538783,
8.37372922300284));
#18662=CARTESIAN_POINT('Ctrl Pts',(-0.068654744322021,-3.1012502399338,
8.42639418666953));
#18663=CARTESIAN_POINT('Ctrl Pts',(1.02005556377276,-2.92949708506828,8.47905915033621));
#18664=CARTESIAN_POINT('Ctrl Pts',(1.78993539631662,-2.34079256521527,8.53172411400289));
#18665=CARTESIAN_POINT('Ctrl Pts',(2.55981522886048,-1.75208804536226,8.58438907766958));
#18666=CARTESIAN_POINT('Ctrl Pts',(3.01086458585342,-0.746432160521719,
8.63705404133626));
#18667=CARTESIAN_POINT('Ctrl Pts',(2.93849705553841,0.220030931794408,8.68971900500295));
#18668=CARTESIAN_POINT('Ctrl Pts',(2.86612952522341,1.18649402411053,8.74238396866963));
#18669=CARTESIAN_POINT('Ctrl Pts',(2.27034510760049,2.11376432390223,8.79504893233632));
#18670=CARTESIAN_POINT('Ctrl Pts',(1.42137896494728,2.58125171077128,8.847713896003));
#18671=CARTESIAN_POINT('Ctrl Pts',(0.572412822294062,3.04873909764032,8.90037885966968));
#18672=CARTESIAN_POINT('Ctrl Pts',(-0.529735045389435,3.05644357158669,
8.95304382333637));
#18673=CARTESIAN_POINT('Ctrl Pts',(-1.38515376586909,2.60087054680792,9.00570878700305));
#18674=CARTESIAN_POINT('Ctrl Pts',(-2.24057248634875,2.14529752202914,9.05837375066974));
#18675=CARTESIAN_POINT('Ctrl Pts',(-2.84926205962455,1.2264469985252,9.11103871433643));
#18676=CARTESIAN_POINT('Ctrl Pts',(-2.93513381881397,0.261090064936974,
9.16370367800311));
#18677=CARTESIAN_POINT('Ctrl Pts',(-2.94280828744918,0.174814884615283,
9.16841041297221));
#18678=CARTESIAN_POINT('Ctrl Pts',(-2.94630689264378,0.0881682471389342,
9.1731171479413));
#18679=CARTESIAN_POINT('Ctrl Pts',(-2.94577110767244,0.00147777103002609,
9.1778238829104));
#18680=CARTESIAN_POINT('Origin',(0.,0.,0.));
#18681=CARTESIAN_POINT('',(-2.93735377875815,0.0004158914717875,10.3221761170896));
#18682=CARTESIAN_POINT('',(-2.93779053274574,0.00122895754932335,10.1778238829104));
#18683=CARTESIAN_POINT('',(-2.942,-3.60291088309151E-16,0.));
#18684=CARTESIAN_POINT('Ctrl Pts',(-2.93735377875815,0.0004158914717875,
10.3221761170896));
#18685=CARTESIAN_POINT('Ctrl Pts',(-2.93794360094505,0.462502223744089,
10.2972708958728));
#18686=CARTESIAN_POINT('Ctrl Pts',(-2.83526550161259,0.924340675123848,
10.2723656746559));
#18687=CARTESIAN_POINT('Ctrl Pts',(-2.6279195904465,1.33308353810155,10.2474604534391));
#18688=CARTESIAN_POINT('Ctrl Pts',(-2.18983399605069,2.19668561771623,10.1948400830687));
#18689=CARTESIAN_POINT('Ctrl Pts',(-1.28450826872579,2.82326745826868,10.1422197126983));
#18690=CARTESIAN_POINT('Ctrl Pts',(-0.321941779407734,2.9290658210569,10.0895993423279));
#18691=CARTESIAN_POINT('Ctrl Pts',(0.640624709910309,3.03486418384512,10.0369789719576));
#18692=CARTESIAN_POINT('Ctrl Pts',(1.66043196122149,2.61987906886913,9.98435860158721));
#18693=CARTESIAN_POINT('Ctrl Pts',(2.27563478565877,1.87204685190273,9.93173823121684));
#18694=CARTESIAN_POINT('Ctrl Pts',(2.89083761009605,1.12421463493634,9.87911786084647));
#18695=CARTESIAN_POINT('Ctrl Pts',(3.10143600765941,0.0435353159795382,
9.82649749047609));
#18696=CARTESIAN_POINT('Ctrl Pts',(2.8120552331994,-0.880578479665677,9.77387712010572));
#18697=CARTESIAN_POINT('Ctrl Pts',(2.52267445873939,-1.8046922753109,9.72125674973535));
#18698=CARTESIAN_POINT('Ctrl Pts',(1.733314512256,-2.57224054764455,9.66863637936499));
#18699=CARTESIAN_POINT('Ctrl Pts',(0.801456763974427,-2.83561988794246,
9.61601600899462));
#18700=CARTESIAN_POINT('Ctrl Pts',(-0.130400984307143,-3.09899922824038,
9.56339563862425));
#18701=CARTESIAN_POINT('Ctrl Pts',(-1.20475653438691,-2.85820963650256,
9.51077526825387));
#18702=CARTESIAN_POINT('Ctrl Pts',(-1.93506113766943,-2.22229869434726,
9.4581548978835));
#18703=CARTESIAN_POINT('Ctrl Pts',(-2.5641326605009,-1.67453620870937,9.41282863761886));
#18704=CARTESIAN_POINT('Ctrl Pts',(-2.93792539338528,-0.833601734574448,
9.36750237735423));
#18705=CARTESIAN_POINT('Ctrl Pts',(-2.94464008512449,0.00207742171232136,
9.3221761170896));
#18706=CARTESIAN_POINT('Ctrl Pts',(-2.94577110767244,0.00147777103002609,
9.1778238829104));
#18707=CARTESIAN_POINT('Ctrl Pts',(-2.94031184592155,-0.881835546255158,
9.22578211160798));
#18708=CARTESIAN_POINT('Ctrl Pts',(-2.51599664630944,-1.76970025068938,
9.27374034030557));
#18709=CARTESIAN_POINT('Ctrl Pts',(-1.82248510748737,-2.31554023703778,
9.32169856900316));
#18710=CARTESIAN_POINT('Ctrl Pts',(-1.06091069186834,-2.91495026175178,
9.37436353266984));
#18711=CARTESIAN_POINT('Ctrl Pts',(0.0252920844727601,-3.1019069675073,
9.42702849633653));
#18712=CARTESIAN_POINT('Ctrl Pts',(0.943444704192239,-2.79161076199491,
9.47969346000322));
#18713=CARTESIAN_POINT('Ctrl Pts',(1.86159732391172,-2.48131455648253,9.5323584236699));
#18714=CARTESIAN_POINT('Ctrl Pts',(2.61169978700958,-1.67376543970224,9.58502338733658));
#18715=CARTESIAN_POINT('Ctrl Pts',(2.85352154222556,-0.735250545330611,
9.63768835100327));
#18716=CARTESIAN_POINT('Ctrl Pts',(3.09534329744155,0.203264349041017,9.69035331466995));
#18717=CARTESIAN_POINT('Ctrl Pts',(2.82888434477565,1.27274502100399,9.74301827833664));
#18718=CARTESIAN_POINT('Ctrl Pts',(2.17500480776272,1.98809774472063,9.79568324200333));
#18719=CARTESIAN_POINT('Ctrl Pts',(1.52112527074978,2.70345046843728,9.84834820567001));
#18720=CARTESIAN_POINT('Ctrl Pts',(0.479825149389799,3.06467524390761,9.90101316933669));
#18721=CARTESIAN_POINT('Ctrl Pts',(-0.476583929910364,2.90792818241875,
9.95367813300337));
#18722=CARTESIAN_POINT('Ctrl Pts',(-1.43299300921054,2.75118112092989,10.0063430966701));
#18723=CARTESIAN_POINT('Ctrl Pts',(-2.3045110464509,2.07646222248183,10.0590080603367));
#18724=CARTESIAN_POINT('Ctrl Pts',(-2.69583596380714,1.18980965393578,10.1116730240034));
#18725=CARTESIAN_POINT('Ctrl Pts',(-2.85967973895049,0.818577213506006,
10.1337233103058));
#18726=CARTESIAN_POINT('Ctrl Pts',(-2.93934508420187,0.410192546500391,
10.1557735966081));
#18727=CARTESIAN_POINT('Ctrl Pts',(-2.93779053274574,0.00122895754932335,
10.1778238829104));
#18728=CARTESIAN_POINT('Origin',(0.,0.,0.));
#18729=CARTESIAN_POINT('',(-2.94318142996902,-0.00248705772575741,11.3221761170896));
#18730=CARTESIAN_POINT('',(-2.94145083142593,-0.00261642954227547,11.1778238829104));
#18731=CARTESIAN_POINT('',(-2.942,-3.60291088309151E-16,0.));
#18732=CARTESIAN_POINT('Ctrl Pts',(-2.94318142996902,-0.00248705772575741,
11.3221761170896));
#18733=CARTESIAN_POINT('Ctrl Pts',(-2.93613735245544,0.782394524444463,
11.2796597847616));
#18734=CARTESIAN_POINT('Ctrl Pts',(-2.61204283140731,1.57241444895454,11.2371434524337));
#18735=CARTESIAN_POINT('Ctrl Pts',(-2.04999848462302,2.11673789269853,11.1946271201057));
#18736=CARTESIAN_POINT('Ctrl Pts',(-1.35438388023453,2.79042020824128,11.1420067497354));
#18737=CARTESIAN_POINT('Ctrl Pts',(-0.294282642636005,3.08774972424349,
11.089386379365));
#18738=CARTESIAN_POINT('Ctrl Pts',(0.65021190135765,2.87407334222539,11.0367660089946));
#18739=CARTESIAN_POINT('Ctrl Pts',(1.59470644535131,2.66039696020728,10.9841456386242));
#18740=CARTESIAN_POINT('Ctrl Pts',(2.42359429574009,1.93571468016887,10.9315252682539));
#18741=CARTESIAN_POINT('Ctrl Pts',(2.76149288344003,1.02821697529914,10.8789048978835));
#18742=CARTESIAN_POINT('Ctrl Pts',(3.09939147113997,0.120719270429434,10.8262845275131));
#18743=CARTESIAN_POINT('Ctrl Pts',(2.9463007961511,-0.969593859271576,10.7736641571428));
#18744=CARTESIAN_POINT('Ctrl Pts',(2.37155179497663,-1.74894687658982,10.7210437867724));
#18745=CARTESIAN_POINT('Ctrl Pts',(1.79680279380215,-2.52829989390807,10.668423416402));
#18746=CARTESIAN_POINT('Ctrl Pts',(0.800395466442055,-2.99669279884355,
10.6158030460317));
#18747=CARTESIAN_POINT('Ctrl Pts',(-0.166422238380945,-2.94200216382593,
10.5631826756613));
#18748=CARTESIAN_POINT('Ctrl Pts',(-1.13323994320395,-2.8873115288083,10.5105623052909));
#18749=CARTESIAN_POINT('Ctrl Pts',(-2.07046802548985,-2.30953735383759,
10.4579419349205));
#18750=CARTESIAN_POINT('Ctrl Pts',(-2.55365933589945,-1.47033910701379,
10.4053215645502));
#18751=CARTESIAN_POINT('Ctrl Pts',(-2.80815619982173,-1.02833338914462,
10.3776064153966));
#18752=CARTESIAN_POINT('Ctrl Pts',(-2.93669740996939,-0.513805263571333,
10.3498912662431));
#18753=CARTESIAN_POINT('Ctrl Pts',(-2.93735377875815,0.0004158914717875,
10.3221761170896));
#18754=CARTESIAN_POINT('Ctrl Pts',(-2.93779053274574,0.00122895754932335,
10.1778238829104));
#18755=CARTESIAN_POINT('Ctrl Pts',(-2.93563218928374,-0.566577199606596,
10.2084385602748));
#18756=CARTESIAN_POINT('Ctrl Pts',(-2.77690932929649,-1.13549932265473,
10.2390532376391));
#18757=CARTESIAN_POINT('Ctrl Pts',(-2.46954008606165,-1.60765366907442,
10.2696679150035));
#18758=CARTESIAN_POINT('Ctrl Pts',(-1.94078749348779,-2.41987818489459,
10.3223328786702));
#18759=CARTESIAN_POINT('Ctrl Pts',(-0.972150510867944,-2.9457409778909,
10.3749978423368));
#18760=CARTESIAN_POINT('Ctrl Pts',(-0.00298230764251388,-2.94672185015728,
10.4276628060035));
#18761=CARTESIAN_POINT('Ctrl Pts',(0.966185895582889,-2.94770272242366,
10.4803277696702));
#18762=CARTESIAN_POINT('Ctrl Pts',(1.93588531941386,-2.42380167396015,10.5329927333369));
#18763=CARTESIAN_POINT('Ctrl Pts',(2.46628089363149,-1.61264909700348,10.5856576970036));
#18764=CARTESIAN_POINT('Ctrl Pts',(2.99667646784912,-0.801496520046785,
10.6383226606703));
#18765=CARTESIAN_POINT('Ctrl Pts',(3.08776819245338,0.296907585403119,10.690987624337));
#18766=CARTESIAN_POINT('Ctrl Pts',(2.69823879520542,1.18435043817229,10.7436525880036));
#18767=CARTESIAN_POINT('Ctrl Pts',(2.30870939795745,2.07179329094149,10.7963175516703));
#18768=CARTESIAN_POINT('Ctrl Pts',(1.43855887885726,2.74827489102996,10.848982515337));
#18769=CARTESIAN_POINT('Ctrl Pts',(0.482469038528927,2.90695754754173,10.9016474790037));
#18770=CARTESIAN_POINT('Ctrl Pts',(-0.473620801799363,3.0656402040535,10.9543124426704));
#18771=CARTESIAN_POINT('Ctrl Pts',(-1.51564996335577,2.70652391698861,11.0069774063371));
#18772=CARTESIAN_POINT('Ctrl Pts',(-2.17097614256679,1.99249620947818,11.0596423700038));
#18773=CARTESIAN_POINT('Ctrl Pts',(-2.66116565955863,1.45839745352016,11.0990362076393));
#18774=CARTESIAN_POINT('Ctrl Pts',(-2.93498842496261,0.725719853723158,
11.1384300452748));
#18775=CARTESIAN_POINT('Ctrl Pts',(-2.94145083142593,-0.00261642954227547,
11.1778238829104));
#18776=CARTESIAN_POINT('Origin',(0.,0.,0.));
#18777=CARTESIAN_POINT('',(-2.9445363666432,0.00211803469319205,12.3221761170896));
#18778=CARTESIAN_POINT('',(-2.94599368555865,0.00130075687149912,12.1778238829104));
#18779=CARTESIAN_POINT('',(-2.942,-3.60291088309151E-16,0.));
#18780=CARTESIAN_POINT('Ctrl Pts',(-2.9445363666432,0.00211803469319205,
12.3221761170896));
#18781=CARTESIAN_POINT('Ctrl Pts',(-2.9456637214079,0.140538485345201,12.3146690440209));
#18782=CARTESIAN_POINT('Ctrl Pts',(-2.93673667551181,0.278812877817704,
12.3071619709522));
#18783=CARTESIAN_POINT('Ctrl Pts',(-2.91725274860024,0.415583368023806,
12.2996548978835));
#18784=CARTESIAN_POINT('Ctrl Pts',(-2.78068135240184,1.37426776932391,12.2470345275131));
#18785=CARTESIAN_POINT('Ctrl Pts',(-2.12542680364205,2.25906209195984,12.1944141571428));
#18786=CARTESIAN_POINT('Ctrl Pts',(-1.24823752065428,2.66926510338839,12.1417937867724));
#18787=CARTESIAN_POINT('Ctrl Pts',(-0.371048237666502,3.07946811481694,
12.089173416402));
#18788=CARTESIAN_POINT('Ctrl Pts',(0.728075779549269,3.01507981503809,12.0365530460316));
#18789=CARTESIAN_POINT('Ctrl Pts',(1.55136877770631,2.50526006508935,11.9839326756613));
#18790=CARTESIAN_POINT('Ctrl Pts',(2.37466177586334,1.99544031514062,11.9313123052909));
#18791=CARTESIAN_POINT('Ctrl Pts',(2.92212375496165,1.04018911502201,11.8786919349205));
#18792=CARTESIAN_POINT('Ctrl Pts',(2.9458228744686,0.0721158274039949,11.8260715645502));
#18793=CARTESIAN_POINT('Ctrl Pts',(2.96952199397554,-0.895957460214037,
11.7734511941798));
#18794=CARTESIAN_POINT('Ctrl Pts',(2.4694582538911,-1.87685283533148,11.7208308238094));
#18795=CARTESIAN_POINT('Ctrl Pts',(1.67209801460167,-2.42634732122405,11.6682104534391));
#18796=CARTESIAN_POINT('Ctrl Pts',(0.874737775312261,-2.9758418071166,11.6155900830687));
#18797=CARTESIAN_POINT('Ctrl Pts',(-0.219918963182118,-3.09393540378431,
11.5629697126983));
#18798=CARTESIAN_POINT('Ctrl Pts',(-1.11612955404462,-2.72714647754463,
11.510349342328));
#18799=CARTESIAN_POINT('Ctrl Pts',(-2.01234014490716,-2.36035755130494,
11.4577289719576));
#18800=CARTESIAN_POINT('Ctrl Pts',(-2.7101045881378,-1.50868610215784,11.4051086015872));
#18801=CARTESIAN_POINT('Ctrl Pts',(-2.89342282416388,-0.557832820042644,
11.3524882312168));
#18802=CARTESIAN_POINT('Ctrl Pts',(-2.9286231547134,-0.375252240171749,
11.3423841931744));
#18803=CARTESIAN_POINT('Ctrl Pts',(-2.94485546023631,-0.189014750280763,
11.332280155132));
#18804=CARTESIAN_POINT('Ctrl Pts',(-2.94318142996902,-0.00248705772575741,
11.3221761170896));
#18805=CARTESIAN_POINT('Ctrl Pts',(-2.94145083142593,-0.00261642954227547,
11.1778238829104));
#18806=CARTESIAN_POINT('Ctrl Pts',(-2.94362790824268,-0.247980760321293,
11.1910950089415));
#18807=CARTESIAN_POINT('Ctrl Pts',(-2.9154621622164,-0.492852393533084,
11.2043661349727));
#18808=CARTESIAN_POINT('Ctrl Pts',(-2.85500395443405,-0.729473081400432,
11.2176372610038));
#18809=CARTESIAN_POINT('Ctrl Pts',(-2.61508239022462,-1.6684755368126,11.2703022246705));
#18810=CARTESIAN_POINT('Ctrl Pts',(-1.86661606494013,-2.4775413196809,11.3229671883372));
#18811=CARTESIAN_POINT('Ctrl Pts',(-0.949093412422085,-2.7896953688222,
11.3756321520039));
#18812=CARTESIAN_POINT('Ctrl Pts',(-0.0315707599040525,-3.10184941796349,
11.4282971156705));
#18813=CARTESIAN_POINT('Ctrl Pts',(1.05500821984753,-2.91709173337779,11.4809620793372));
#18814=CARTESIAN_POINT('Ctrl Pts',(1.81779437152408,-2.31922447800469,11.5336270430039));
#18815=CARTESIAN_POINT('Ctrl Pts',(2.58058052320064,-1.7213572226316,11.5862920066706));
#18816=CARTESIAN_POINT('Ctrl Pts',(3.01957384680218,-0.710380396471107,
11.6389569703373));
#18817=CARTESIAN_POINT('Ctrl Pts',(2.93565629151018,0.255148376847553,11.691621934004));
#18818=CARTESIAN_POINT('Ctrl Pts',(2.85173873621817,1.22067715016623,11.7442868976707));
#18819=CARTESIAN_POINT('Ctrl Pts',(2.24491030203262,2.14075787064307,11.7969518613373));
#18820=CARTESIAN_POINT('Ctrl Pts',(1.39041548234847,2.59806145861508,11.849616825004));
#18821=CARTESIAN_POINT('Ctrl Pts',(0.535920662664327,3.05536504658708,11.9022817886707));
#18822=CARTESIAN_POINT('Ctrl Pts',(-0.566240542518395,3.04989150205426,
11.9549467523374));
#18823=CARTESIAN_POINT('Ctrl Pts',(-1.41615121076395,2.58412350821102,12.0076117160041));
#18824=CARTESIAN_POINT('Ctrl Pts',(-2.26606187900951,2.11835551436778,12.0602766796708));
#18825=CARTESIAN_POINT('Ctrl Pts',(-2.86372201031791,1.19229307121411,12.1129416433374));
#18826=CARTESIAN_POINT('Ctrl Pts',(-2.93804565964555,0.22597844177242,12.1656066070041));
#18827=CARTESIAN_POINT('Ctrl Pts',(-2.94379288681505,0.151256200025011,
12.1696790323062));
#18828=CARTESIAN_POINT('Ctrl Pts',(-2.94641083929854,0.0762932715455572,
12.1737514576083));
#18829=CARTESIAN_POINT('Ctrl Pts',(-2.94599368555865,0.00130075687149912,
12.1778238829104));
#18830=CARTESIAN_POINT('Origin',(0.,0.,0.));
#18831=CARTESIAN_POINT('',(-2.93733773658367,0.000353650820144602,13.3221761170896));
#18832=CARTESIAN_POINT('',(-2.93794966127546,0.0013934910171998,13.1778238829104));
#18833=CARTESIAN_POINT('',(-2.942,-3.60291088309151E-16,0.));
#18834=CARTESIAN_POINT('Ctrl Pts',(-2.93733773658367,0.000353650820144602,
13.3221761170896));
#18835=CARTESIAN_POINT('Ctrl Pts',(-2.93784318272048,0.466397170874405,
13.2970579329098));
#18836=CARTESIAN_POINT('Ctrl Pts',(-2.8333193685149,0.932226520914598,13.27193974873));
#18837=CARTESIAN_POINT('Ctrl Pts',(-2.62254748003497,1.34362161549686,13.2468215645502));
#18838=CARTESIAN_POINT('Ctrl Pts',(-2.18099904818651,2.20545788879211,13.1942011941798));
#18839=CARTESIAN_POINT('Ctrl Pts',(-1.27316460447925,2.82840106158337,13.1415808238094));
#18840=CARTESIAN_POINT('Ctrl Pts',(-0.31018098965669,2.93033473129373,13.0889604534391));
#18841=CARTESIAN_POINT('Ctrl Pts',(0.652802625165875,3.03226840100409,13.0363400830687));
#18842=CARTESIAN_POINT('Ctrl Pts',(1.67093541110377,2.61319256763355,12.9837197126983));
#18843=CARTESIAN_POINT('Ctrl Pts',(2.28313120153524,1.86289672775273,12.9310993423279));
#18844=CARTESIAN_POINT('Ctrl Pts',(2.89532699196672,1.1126008878719,12.8784789719576));
#18845=CARTESIAN_POINT('Ctrl Pts',(3.10158578689178,0.0310850414808014,
12.8258586015872));
#18846=CARTESIAN_POINT('Ctrl Pts',(2.80849777284497,-0.891859624755379,
12.7732382312168));
#18847=CARTESIAN_POINT('Ctrl Pts',(2.51540975879817,-1.81480429099155,12.7206178608465));
#18848=CARTESIAN_POINT('Ctrl Pts',(1.72297493577951,-2.57917777707278,12.6679974904761));
#18849=CARTESIAN_POINT('Ctrl Pts',(0.790067400131255,-2.83881430845519,
12.6153771201057));
#18850=CARTESIAN_POINT('Ctrl Pts',(-0.142840135516982,-3.0984508398376,
12.5627567497353));
#18851=CARTESIAN_POINT('Ctrl Pts',(-1.21622038379481,-2.85335041652122,
12.510136379365));
#18852=CARTESIAN_POINT('Ctrl Pts',(-1.94396638611522,-2.21451296488091,
12.4575160089946));
#18853=CARTESIAN_POINT('Ctrl Pts',(-2.56788867194677,-1.66681511174075,
12.4124027116929));
#18854=CARTESIAN_POINT('Ctrl Pts',(-2.93776159700942,-0.829711212970877,
12.3672894143913));
#18855=CARTESIAN_POINT('Ctrl Pts',(-2.9445363666432,0.00211803469319205,
12.3221761170896));
#18856=CARTESIAN_POINT('Ctrl Pts',(-2.94599368555865,0.00130075687149912,
12.1778238829104));
#18857=CARTESIAN_POINT('Ctrl Pts',(-2.94101617029297,-0.893516551252978,
12.226416421275));
#18858=CARTESIAN_POINT('Ctrl Pts',(-2.50391622116005,-1.79254618589271,
12.2750089596396));
#18859=CARTESIAN_POINT('Ctrl Pts',(-1.79466984706922,-2.33716467042755,
12.3236014980042));
#18860=CARTESIAN_POINT('Ctrl Pts',(-1.02598321781837,-2.92742633745608,
12.3762664616709));
#18861=CARTESIAN_POINT('Ctrl Pts',(0.0623772080302214,-3.10138285578342,
12.4289314253375));
#18862=CARTESIAN_POINT('Ctrl Pts',(0.976754244976282,-2.78013123936204,
12.4815963890042));
#18863=CARTESIAN_POINT('Ctrl Pts',(1.89113128192235,-2.45887962294065,12.5342613526709));
#18864=CARTESIAN_POINT('Ctrl Pts',(2.6315249299659,-1.64241987177053,12.5869263163376));
#18865=CARTESIAN_POINT('Ctrl Pts',(2.86210835815027,-0.701080799331296,
12.6395912800043));
#18866=CARTESIAN_POINT('Ctrl Pts',(3.09269178633465,0.240258273107937,12.692256243671));
#18867=CARTESIAN_POINT('Ctrl Pts',(2.81346499465986,1.30647666681628,12.7449212073377));
#18868=CARTESIAN_POINT('Ctrl Pts',(2.15107931219979,2.01396036610533,12.7975861710043));
#18869=CARTESIAN_POINT('Ctrl Pts',(1.48869362973973,2.72144406539436,12.850251134671));
#18870=CARTESIAN_POINT('Ctrl Pts',(0.443149056494409,3.07019307026412,12.9029160983377));
#18871=CARTESIAN_POINT('Ctrl Pts',(-0.511317558922748,2.90202221756343,
12.9555810620044));
#18872=CARTESIAN_POINT('Ctrl Pts',(-1.46578417433991,2.73385136486274,13.0082460256711));
#18873=CARTESIAN_POINT('Ctrl Pts',(-2.3291728319289,2.04876065459161,13.0609109893378));
#18874=CARTESIAN_POINT('Ctrl Pts',(-2.7098688231833,1.1574927237348,13.1135759530044));
#18875=CARTESIAN_POINT('Ctrl Pts',(-2.86467717936984,0.795062526234979,
13.1349919296398));
#18876=CARTESIAN_POINT('Ctrl Pts',(-2.93966715879244,0.398538727939818,
13.1564079062751));
#18877=CARTESIAN_POINT('Ctrl Pts',(-2.93794966127546,0.0013934910171998,
13.1778238829104));
#18878=CARTESIAN_POINT('Origin',(0.,0.,0.));
#18879=CARTESIAN_POINT('',(-2.94325266537063,-0.0024318079996577,14.3221761170896));
#18880=CARTESIAN_POINT('',(-2.94111188951679,-0.00259486169482749,14.1778238829104));
#18881=CARTESIAN_POINT('',(-2.942,-3.60291088309151E-16,0.));
#18882=CARTESIAN_POINT('Ctrl Pts',(-2.94325266537063,-0.0024318079996577,
14.3221761170896));
#18883=CARTESIAN_POINT('Ctrl Pts',(-2.93620194204164,0.786300619982285,
14.2794468217987));
#18884=CARTESIAN_POINT('Ctrl Pts',(-2.60854122084458,1.58016790859219,14.2367175265078));
#18885=CARTESIAN_POINT('Ctrl Pts',(-2.04150376744995,2.12493551247607,14.1939882312168));
#18886=CARTESIAN_POINT('Ctrl Pts',(-1.34320718641939,2.79580716825642,14.1413678608465));
#18887=CARTESIAN_POINT('Ctrl Pts',(-0.281884150596186,3.08890703892681,
14.0887474904761));
#18888=CARTESIAN_POINT('Ctrl Pts',(0.661753798897932,2.87144767774516,14.0361271201057));
#18889=CARTESIAN_POINT('Ctrl Pts',(1.60539174839208,2.65398831656351,13.9835067497354));
#18890=CARTESIAN_POINT('Ctrl Pts',(2.43134461155714,1.92596972352975,13.930886379365));
#18891=CARTESIAN_POINT('Ctrl Pts',(2.76559296922098,1.01711939779235,13.8782660089946));
#18892=CARTESIAN_POINT('Ctrl Pts',(3.09984132688481,0.108269072054953,13.8256456386242));
#18893=CARTESIAN_POINT('Ctrl Pts',(2.94238517904746,-0.981412986386104,
13.7730252682539));
#18894=CARTESIAN_POINT('Ctrl Pts',(2.36451469520878,-1.75845069530582,13.7204048978835));
#18895=CARTESIAN_POINT('Ctrl Pts',(1.7866442113701,-2.53548840422553,13.6677845275131));
#18896=CARTESIAN_POINT('Ctrl Pts',(0.788359391530092,-2.99988176362388,
13.6151641571428));
#18897=CARTESIAN_POINT('Ctrl Pts',(-0.178232238982059,-2.94131149038551,
13.5625437867724));
#18898=CARTESIAN_POINT('Ctrl Pts',(-1.14482386949421,-2.88274121714715,
13.509923416402));
#18899=CARTESIAN_POINT('Ctrl Pts',(-2.07972231067849,-2.30120731127206,
13.4573030460317));
#18900=CARTESIAN_POINT('Ctrl Pts',(-2.5595403212758,-1.46007567143488,13.4046826756613));
#18901=CARTESIAN_POINT('Ctrl Pts',(-2.81031856879004,-1.02045582826861,
13.3771804894707));
#18902=CARTESIAN_POINT('Ctrl Pts',(-2.9367843178467,-0.509922711901109,
13.3496783032802));
#18903=CARTESIAN_POINT('Ctrl Pts',(-2.93733773658367,0.000353650820144602,
13.3221761170896));
#18904=CARTESIAN_POINT('Ctrl Pts',(-2.93794966127546,0.0013934910171998,
13.1778238829104));
#18905=CARTESIAN_POINT('Ctrl Pts',(-2.9354435856223,-0.578098472832708,
13.2090728699418));
#18906=CARTESIAN_POINT('Ctrl Pts',(-2.76961959866241,-1.15891354184382,
13.2403218569731));
#18907=CARTESIAN_POINT('Ctrl Pts',(-2.45014221851649,-1.63706498032062,
13.2715708440045));
#18908=CARTESIAN_POINT('Ctrl Pts',(-1.91171629767549,-2.44290960207673,
13.3242358076712));
#18909=CARTESIAN_POINT('Ctrl Pts',(-0.936861131073665,-2.95715369414646,
13.3769007713379));
#18910=CARTESIAN_POINT('Ctrl Pts',(0.032249473718084,-2.94654692146698,
13.4295657350046));
#18911=CARTESIAN_POINT('Ctrl Pts',(1.00136007850986,-2.9359401487875,13.4822306986712));
#18912=CARTESIAN_POINT('Ctrl Pts',(1.96472612149158,-2.40048251135878,13.5348956623379));
#18913=CARTESIAN_POINT('Ctrl Pts',(2.48538560527679,-1.58304647931889,13.5875606260046));
#18914=CARTESIAN_POINT('Ctrl Pts',(3.00604508906198,-0.765610447279041,
13.6402255896713));
#18915=CARTESIAN_POINT('Ctrl Pts',(3.08399801365073,0.333803979371919,13.692890553338));
#18916=CARTESIAN_POINT('Ctrl Pts',(2.68388585052197,1.21652624548705,13.7455555170047));
#18917=CARTESIAN_POINT('Ctrl Pts',(2.28377368739319,2.0992485116022,13.7982204806713));
#18918=CARTESIAN_POINT('Ctrl Pts',(1.40559643654686,2.76527861718149,13.850885444338));
#18919=CARTESIAN_POINT('Ctrl Pts',(0.447678061833244,2.91251851826326,13.9035504080047));
#18920=CARTESIAN_POINT('Ctrl Pts',(-0.510240312880357,3.05975841934504,
13.9562153716714));
#18921=CARTESIAN_POINT('Ctrl Pts',(-1.54789981146125,2.68820811592931,14.0088803353381));
#18922=CARTESIAN_POINT('Ctrl Pts',(-2.1946428070508,1.96639671204873,14.0615452990048));
#18923=CARTESIAN_POINT('Ctrl Pts',(-2.67062249982462,1.435169358057,14.1003048269733));
#18924=CARTESIAN_POINT('Ctrl Pts',(-2.93486488519192,0.714225423327012,
14.1390643549419));
#18925=CARTESIAN_POINT('Ctrl Pts',(-2.94111188951679,-0.00259486169482749,
14.1778238829104));
#18926=CARTESIAN_POINT('Origin',(0.,0.,-1.84858989190501));
#18927=CARTESIAN_POINT('',(-2.37275986033066,-0.00196044888638088,14.651410108095));
#18928=CARTESIAN_POINT('',(-2.37517539399571,0.0009292342096269,14.848589891905));
#18929=CARTESIAN_POINT('',(-2.37175,-2.62313128856983E-13,-1.84858989190501));
#18930=CARTESIAN_POINT('',(-2.34668236863853,0.343918483395512,15.62825));
#18931=CARTESIAN_POINT('Ctrl Pts',(-2.37275986033066,-0.00196044888638126,
14.651410108095));
#18932=CARTESIAN_POINT('Ctrl Pts',(-2.37407562336888,-0.149148890039704,
14.6613011831744));
#18933=CARTESIAN_POINT('Ctrl Pts',(-2.29486163858049,-1.07797575416432,
14.7238126286243));
#18934=CARTESIAN_POINT('Ctrl Pts',(-1.07036982067409,-2.58532778276268,
14.8389444444444));
#18935=CARTESIAN_POINT('Ctrl Pts',(1.57881200919325,-2.30987053095853,14.9968055555556));
#18936=CARTESIAN_POINT('Ctrl Pts',(2.79654399706859,0.0566462213665858,
15.1546666666667));
#18937=CARTESIAN_POINT('Ctrl Pts',(1.48409012818578,2.37398300468726,15.3125277777778));
#18938=CARTESIAN_POINT('Ctrl Pts',(-1.17817012667699,2.53688639776398,15.4703888888889));
#18939=CARTESIAN_POINT('Ctrl Pts',(-2.23297482288527,1.11978691060522,15.5756296296296));
#18940=CARTESIAN_POINT('Ctrl Pts',(-2.34668236863854,0.343918483395395,
15.62825));
#18941=CARTESIAN_POINT('',(-0.439445221994505,2.33068358199182,15.62825));
#18942=CARTESIAN_POINT('Origin',(0.,0.,15.62825));
#18943=CARTESIAN_POINT('Ctrl Pts',(-2.37517539399571,0.000929234209626874,
14.848589891905));
#18944=CARTESIAN_POINT('Ctrl Pts',(-2.37154287511732,-0.72977569986937,
14.8978167399366));
#18945=CARTESIAN_POINT('Ctrl Pts',(-1.620069408967,-2.24871933567263,14.9997085516349));
#18946=CARTESIAN_POINT('Ctrl Pts',(0.958368222991996,-2.62865236842956,
15.1542653269999));
#18947=CARTESIAN_POINT('Ctrl Pts',(2.7277014223945,-0.634378452891388,15.3122602179999));
#18948=CARTESIAN_POINT('Ctrl Pts',(2.01676643438217,1.93930517753648,15.470255109));
#18949=CARTESIAN_POINT('Ctrl Pts',(0.331786659212352,2.47609764328476,15.5755850363333));
#18950=CARTESIAN_POINT('Ctrl Pts',(-0.439445221994538,2.33068358199181,
15.62825));
#18951=CARTESIAN_POINT('Origin',(0.,0.,-1.84858989190501));
#18952=CARTESIAN_POINT('',(-2.36799142649297,0.000285102424211894,13.651410108095));
#18953=CARTESIAN_POINT('',(-2.37103403261776,-0.00209189776527924,13.848589891905));
#18954=CARTESIAN_POINT('',(-2.37175,-2.62313128856983E-13,-1.84858989190501));
#18955=CARTESIAN_POINT('Ctrl Pts',(-2.36799142649297,0.000285102424211897,
13.651410108095));
#18956=CARTESIAN_POINT('Ctrl Pts',(-2.36754527731231,-0.41108402173757,
13.6789122942855));
#18957=CARTESIAN_POINT('Ctrl Pts',(-2.07052456040773,-1.61013525385437,
13.7590348508465));
#18958=CARTESIAN_POINT('Ctrl Pts',(-0.16923542984156,-2.79279215602584,
13.8917777777778));
#18959=CARTESIAN_POINT('Ctrl Pts',(2.24512421134353,-1.66965318578134,14.0496388888889));
#18960=CARTESIAN_POINT('Ctrl Pts',(2.62593313585052,0.965751391486786,14.2075));
#18961=CARTESIAN_POINT('Ctrl Pts',(0.628359679142483,2.72647005025058,14.3653611111111));
#18962=CARTESIAN_POINT('Ctrl Pts',(-1.77762972544941,2.06202090562868,14.5133311471428));
#18963=CARTESIAN_POINT('Ctrl Pts',(-2.36707578383325,0.633891398858792,
14.6086808128041));
#18964=CARTESIAN_POINT('Ctrl Pts',(-2.37275986033066,-0.00196044888638126,
14.651410108095));
#18965=CARTESIAN_POINT('Ctrl Pts',(-2.37103403261776,-0.00209189776527889,
13.848589891905));
#18966=CARTESIAN_POINT('Ctrl Pts',(-2.37284080801943,-0.20941258958213,
13.8624953276032));
#18967=CARTESIAN_POINT('Ctrl Pts',(-2.25333213139831,-1.19988405133594,
13.929065726968));
#18968=CARTESIAN_POINT('Ctrl Pts',(-0.869666078203209,-2.66015561356989,
14.0483010899995));
#18969=CARTESIAN_POINT('Ctrl Pts',(1.75267763866885,-2.18191305067097,14.2062959809995));
#18970=CARTESIAN_POINT('Ctrl Pts',(2.78512620401791,0.275629071355557,14.3642908719996));
#18971=CARTESIAN_POINT('Ctrl Pts',(1.29091271455523,2.48320730756548,14.5222857629997));
#18972=CARTESIAN_POINT('Ctrl Pts',(-1.37414448785656,2.43798182357128,14.6802806539997));
#18973=CARTESIAN_POINT('Ctrl Pts',(-2.35095938458833,0.884486526760038,
14.7890486969682));
#18974=CARTESIAN_POINT('Ctrl Pts',(-2.37542909742077,0.0519633377314283,
14.8451517762699));
#18975=CARTESIAN_POINT('Ctrl Pts',(-2.37517539399571,0.000929234209626874,
14.848589891905));
#18976=CARTESIAN_POINT('Origin',(0.,0.,-1.84858989190501));
#18977=CARTESIAN_POINT('',(-2.3737947408518,0.00170749448784205,12.651410108095));
#18978=CARTESIAN_POINT('',(-2.36848474137664,0.00112338963946246,12.848589891905));
#18979=CARTESIAN_POINT('',(-2.37175,-2.62313128856983E-13,-1.84858989190501));
#18980=CARTESIAN_POINT('Ctrl Pts',(-2.3737947408518,0.00170749448784207,
12.651410108095));
#18981=CARTESIAN_POINT('Ctrl Pts',(-2.36833312974404,-0.668887685031927,
12.6965234053967));
#18982=CARTESIAN_POINT('Ctrl Pts',(-1.72235411599047,-2.13088047848934,
12.7942570730687));
#18983=CARTESIAN_POINT('Ctrl Pts',(0.750172845833004,-2.69546828972993,
12.9446111111111));
#18984=CARTESIAN_POINT('Ctrl Pts',(2.66668266040929,-0.846825037914988,
13.1024722222222));
#18985=CARTESIAN_POINT('Ctrl Pts',(2.16784415239069,1.76882949166842,13.2603333333333));
#18986=CARTESIAN_POINT('Ctrl Pts',(-0.294517949969841,2.78236767093066,
13.4181944444444));
#18987=CARTESIAN_POINT('Ctrl Pts',(-2.10760963637491,1.5382497642797,13.548553369365));
#18988=CARTESIAN_POINT('Ctrl Pts',(-2.36839890163746,0.375995067988055,
13.6262919239152));
#18989=CARTESIAN_POINT('Ctrl Pts',(-2.36799142649297,0.000285102424211897,
13.651410108095));
#18990=CARTESIAN_POINT('Ctrl Pts',(-2.36848474137664,0.00112338963946246,
12.848589891905));
#18991=CARTESIAN_POINT('Ctrl Pts',(-2.36646442019019,-0.466045225337024,
12.8798388789364));
#18992=CARTESIAN_POINT('Ctrl Pts',(-2.00748312661735,-1.72341304420753,
12.9637528296344));
#18993=CARTESIAN_POINT('Ctrl Pts',(0.0306296239850783,-2.7985342282319,
13.1003317439992));
#18994=CARTESIAN_POINT('Ctrl Pts',(2.36053793034993,-1.50352574600393,13.2583266349992));
#18995=CARTESIAN_POINT('Ctrl Pts',(2.54906768788899,1.15541663986578,13.4163215259993));
#18996=CARTESIAN_POINT('Ctrl Pts',(0.42518914129335,2.76621565710669,13.5743164169993));
#18997=CARTESIAN_POINT('Ctrl Pts',(-1.86352481270074,1.94670562977947,13.7184058723013));
#18998=CARTESIAN_POINT('Ctrl Pts',(-2.36599788968529,0.57578658999839,13.8098303639365));
#18999=CARTESIAN_POINT('Ctrl Pts',(-2.37103403261776,-0.00209189776527889,
13.848589891905));
#19000=CARTESIAN_POINT('Origin',(0.,0.,-1.84858989190501));
#19001=CARTESIAN_POINT('',(-2.37270243253876,-0.00200498951788303,11.651410108095));
#19002=CARTESIAN_POINT('',(-2.37496958658182,0.00104863022067879,11.848589891905));
#19003=CARTESIAN_POINT('',(-2.37175,-2.62313128856983E-13,-1.84858989190501));
#19004=CARTESIAN_POINT('Ctrl Pts',(-2.37270243253876,-0.00200498951788284,
11.651410108095));
#19005=CARTESIAN_POINT('Ctrl Pts',(-2.37405198430164,-0.152377883745359,
11.6615141461374));
#19006=CARTESIAN_POINT('Ctrl Pts',(-2.29281607417404,-1.08441874324097,
11.7242385545502));
#19007=CARTESIAN_POINT('Ctrl Pts',(-1.05977053720295,-2.58943908287633,
11.8395833333333));
#19008=CARTESIAN_POINT('Ctrl Pts',(1.58766534266525,-2.30382879610199,11.9974444444444));
#19009=CARTESIAN_POINT('Ctrl Pts',(2.79707340746319,0.0684743370742143,
12.1553055555555));
#19010=CARTESIAN_POINT('Ctrl Pts',(1.47303233105958,2.37875683253439,12.3131666666667));
#19011=CARTESIAN_POINT('Ctrl Pts',(-1.18520769732058,2.53448043892505,12.4710277777778));
#19012=CARTESIAN_POINT('Ctrl Pts',(-2.31706196946124,1.00613052370996,12.5837755915872));
#19013=CARTESIAN_POINT('Ctrl Pts',(-2.37470357962243,0.113297808503467,
12.6439030350263));
#19014=CARTESIAN_POINT('Ctrl Pts',(-2.3737947408518,0.00170749448784207,
12.651410108095));
#19015=CARTESIAN_POINT('Ctrl Pts',(-2.37496958658182,0.00104863022067909,
11.848589891905));
#19016=CARTESIAN_POINT('Ctrl Pts',(-2.37095686672064,-0.72032558818314,
11.8971824302696));
#19017=CARTESIAN_POINT('Ctrl Pts',(-1.63667192852724,-2.23060698037937,
11.9984399323009));
#19018=CARTESIAN_POINT('Ctrl Pts',(0.927689321261817,-2.64047796075702,
12.1523623979988));
#19019=CARTESIAN_POINT('Ctrl Pts',(2.71833714731268,-0.66586366962402,12.3103572889989));
#19020=CARTESIAN_POINT('Ctrl Pts',(2.04302496870488,1.91279385105346,12.468352179999));
#19021=CARTESIAN_POINT('Ctrl Pts',(-0.48563275555883,2.75624604578475,12.626347070999));
#19022=CARTESIAN_POINT('Ctrl Pts',(-2.16074812800628,1.4270578867686,12.7530929749677));
#19023=CARTESIAN_POINT('Ctrl Pts',(-2.36986933510064,0.32128967640745,12.8271739152697));
#19024=CARTESIAN_POINT('Ctrl Pts',(-2.36848474137664,0.00112338963946246,
12.848589891905));
#19025=CARTESIAN_POINT('Origin',(0.,0.,-1.84858989190501));
#19026=CARTESIAN_POINT('',(-2.3680043592011,0.000335278925106314,10.651410108095));
#19027=CARTESIAN_POINT('',(-2.37130727717011,-0.00210928510120167,10.848589891905));
#19028=CARTESIAN_POINT('',(-2.37175,-2.62313128856983E-13,-1.84858989190501));
#19029=CARTESIAN_POINT('Ctrl Pts',(-2.3680043592011,0.000335278925106194,
10.651410108095));
#19030=CARTESIAN_POINT('Ctrl Pts',(-2.36747521485208,-0.414214015593381,
10.6791252572485));
#19031=CARTESIAN_POINT('Ctrl Pts',(-2.06710351553143,-1.61654972761244,
10.7594607767724));
#19032=CARTESIAN_POINT('Ctrl Pts',(-0.158018739337926,-2.79344562132492,
10.8924166666667));
#19033=CARTESIAN_POINT('Ctrl Pts',(2.25180017160661,-1.66063371893121,11.0502777777778));
#19034=CARTESIAN_POINT('Ctrl Pts',(2.62205116590109,0.976297109112734,11.2081388888889));
#19035=CARTESIAN_POINT('Ctrl Pts',(0.617379419647229,2.72894686881467,11.366));
#19036=CARTESIAN_POINT('Ctrl Pts',(-1.78238141625357,2.05587933285381,11.5137570730687));
#19037=CARTESIAN_POINT('Ctrl Pts',(-2.36702371369352,0.630742424660346,
11.608893775767));
#19038=CARTESIAN_POINT('Ctrl Pts',(-2.37270243253876,-0.00200498951788284,
11.651410108095));
#19039=CARTESIAN_POINT('Ctrl Pts',(-2.37130727717011,-0.00210928510120129,
10.848589891905));
#19040=CARTESIAN_POINT('Ctrl Pts',(-2.37306236960384,-0.199914469168129,
10.8618610179362));
#19041=CARTESIAN_POINT('Ctrl Pts',(-2.26024839139859,-1.18071373741556,
10.927797107634));
#19042=CARTESIAN_POINT('Ctrl Pts',(-0.90141796228012,-2.64956165719617,
11.0463981609985));
#19043=CARTESIAN_POINT('Ctrl Pts',(1.72648179491819,-2.20272375262492,11.2043930519985));
#19044=CARTESIAN_POINT('Ctrl Pts',(2.7881905800153,0.242331605070017,11.3623879429986));
#19045=CARTESIAN_POINT('Ctrl Pts',(1.32057126786748,2.46755402056041,11.5203828339987));
#19046=CARTESIAN_POINT('Ctrl Pts',(-1.34501422335496,2.45431621031658,11.6783777249987));
#19047=CARTESIAN_POINT('Ctrl Pts',(-2.34590203170026,0.903460530701682,
11.7877800776342));
#19048=CARTESIAN_POINT('Ctrl Pts',(-2.37530588310888,0.0615052912262518,
11.8445174666029));
#19049=CARTESIAN_POINT('Ctrl Pts',(-2.37496958658182,0.00104863022067909,
11.848589891905));
#19050=CARTESIAN_POINT('Origin',(0.,0.,-1.84858989190501));
#19051=CARTESIAN_POINT('',(-2.37387835550442,0.0016747535505271,9.65141010809499));
#19052=CARTESIAN_POINT('',(-2.36835645684558,0.000990747813277848,9.84858989190503));
#19053=CARTESIAN_POINT('',(-2.37175,-2.62313128856983E-13,-1.84858989190501));
#19054=CARTESIAN_POINT('Ctrl Pts',(-2.37387835550442,0.00167475355052717,
9.65141010809499));
#19055=CARTESIAN_POINT('Ctrl Pts',(-2.36846517734921,-0.672024104003181,
9.69673636835963));
#19056=CARTESIAN_POINT('Ctrl Pts',(-1.71729169385484,-2.1369916722257,9.79468299899462));
#19057=CARTESIAN_POINT('Ctrl Pts',(0.760987165659879,-2.69243512365168,
9.94525));
#19058=CARTESIAN_POINT('Ctrl Pts',(2.6700603672968,-0.836113626465368,10.1031111111111));
#19059=CARTESIAN_POINT('Ctrl Pts',(2.16072649637127,1.7775177549783,10.2609722222222));
#19060=CARTESIAN_POINT('Ctrl Pts',(-0.305685313585232,2.78116249982291,
10.4188333333333));
#19061=CARTESIAN_POINT('Ctrl Pts',(-2.11081288774265,1.53182193243431,10.5489792952909));
#19062=CARTESIAN_POINT('Ctrl Pts',(-2.36847985572451,0.37285508129321,10.6265048868781));
#19063=CARTESIAN_POINT('Ctrl Pts',(-2.3680043592011,0.000335278925106194,
10.651410108095));
#19064=CARTESIAN_POINT('Ctrl Pts',(-2.36835645684558,0.00099074781327764,
9.84858989190503));
#19065=CARTESIAN_POINT('Ctrl Pts',(-2.36661646666674,-0.456757128880904,
9.87920456926939));
#19066=CARTESIAN_POINT('Ctrl Pts',(-2.01853982608692,-1.70439405627733,
9.96248421030043));
#19067=CARTESIAN_POINT('Ctrl Pts',(-0.00283249851198579,-2.79870028674429,
10.0984288149982));
#19068=CARTESIAN_POINT('Ctrl Pts',(2.34239313895008,-1.53164150527581,10.2564237059982));
#19069=CARTESIAN_POINT('Ctrl Pts',(2.56269918704329,1.12485741087042,10.4144185969983));
#19070=CARTESIAN_POINT('Ctrl Pts',(0.458233353927178,2.76093344928963,10.5724134879983));
#19071=CARTESIAN_POINT('Ctrl Pts',(-1.85023633825226,1.96536160231837,10.7171372529672));
#19072=CARTESIAN_POINT('Ctrl Pts',(-2.36609748365237,0.585053046589831,
10.8091960542695));
#19073=CARTESIAN_POINT('Ctrl Pts',(-2.37130727717011,-0.00210928510120129,
10.848589891905));
#19074=CARTESIAN_POINT('Origin',(0.,0.,-1.84858989190501));
#19075=CARTESIAN_POINT('',(-2.37260887298938,-0.00202072084187682,8.65141010809499));
#19076=CARTESIAN_POINT('',(-2.3747901511292,0.00119133359606532,8.84858989190503));
#19077=CARTESIAN_POINT('',(-2.37175,-2.62313128856983E-13,-1.84858989190501));
#19078=CARTESIAN_POINT('Ctrl Pts',(-2.37260887298937,-0.00202072084187674,
8.65141010809499));
#19079=CARTESIAN_POINT('Ctrl Pts',(-2.37399141457934,-0.155578652695773,
8.66172710910036));
#19080=CARTESIAN_POINT('Ctrl Pts',(-2.29073220490892,-1.09084435213441,
8.72466448047611));
#19081=CARTESIAN_POINT('Ctrl Pts',(-1.04936735270146,-2.59367240037321,
8.84022222222223));
#19082=CARTESIAN_POINT('Ctrl Pts',(1.59690068918271,-2.29743695240177,8.99808333333332));
#19083=CARTESIAN_POINT('Ctrl Pts',(2.79677599470576,0.0797019247629725,
9.15594444444445));
#19084=CARTESIAN_POINT('Ctrl Pts',(1.46347155312646,2.38465078671139,9.31380555555555));
#19085=CARTESIAN_POINT('Ctrl Pts',(-1.19537219008389,2.52970229247383,9.47166666666666));
#19086=CARTESIAN_POINT('Ctrl Pts',(-2.31895585283185,0.999716542450464,
9.58420151751315));
#19087=CARTESIAN_POINT('Ctrl Pts',(-2.37474946901026,0.110089469797055,
9.64411599798926));
#19088=CARTESIAN_POINT('Ctrl Pts',(-2.37387835550442,0.00167475355052717,
9.65141010809499));
#19089=CARTESIAN_POINT('Ctrl Pts',(-2.3747901511292,0.00119133359606537,
8.84858989190503));
#19090=CARTESIAN_POINT('Ctrl Pts',(-2.37038906205444,-0.71090872088079,
8.89654812060261));
#19091=CARTESIAN_POINT('Ctrl Pts',(-1.65267775677864,-2.21269450774448,
8.99717131296688));
#19092=CARTESIAN_POINT('Ctrl Pts',(0.896053003445084,-2.6513808351669,9.15045946899784));
#19093=CARTESIAN_POINT('Ctrl Pts',(2.71018167460651,-0.698316982967359,
9.30845435999788));
#19094=CARTESIAN_POINT('Ctrl Pts',(2.06574861445826,1.88823038317285,9.46644925099794));
#19095=CARTESIAN_POINT('Ctrl Pts',(-0.45264386973844,2.76185532663481,9.62444414199799));
#19096=CARTESIAN_POINT('Ctrl Pts',(-2.15199374797492,1.44623886325989,9.75182435563369));
#19097=CARTESIAN_POINT('Ctrl Pts',(-2.36960968846224,0.330684626839437,
9.8265396056027));
#19098=CARTESIAN_POINT('Ctrl Pts',(-2.36835645684558,0.00099074781327764,
9.84858989190503));
#19099=CARTESIAN_POINT('Origin',(0.,0.,-1.84858989190501));
#19100=CARTESIAN_POINT('',(-2.36801892187683,0.000385579322849399,7.65141010809499));
#19101=CARTESIAN_POINT('',(-2.37158591103805,-0.00211396583053219,7.84858989190503));
#19102=CARTESIAN_POINT('',(-2.37175,-2.62313128856983E-13,-1.84858989190501));
#19103=CARTESIAN_POINT('Ctrl Pts',(-2.36801892187683,0.000385579322849869,
7.65141010809499));
#19104=CARTESIAN_POINT('Ctrl Pts',(-2.36740549965901,-0.417342685994756,
7.67933822021147));
#19105=CARTESIAN_POINT('Ctrl Pts',(-2.06366306314178,-1.62296175556451,
7.75988670269832));
#19106=CARTESIAN_POINT('Ctrl Pts',(-0.146803886877873,-2.79405744038503,
7.89305555555557));
#19107=CARTESIAN_POINT('Ctrl Pts',(2.25844822171206,-1.65158105802259,8.05091666666665));
#19108=CARTESIAN_POINT('Ctrl Pts',(2.61811094239596,0.986814802625037,8.20877777777778));
#19109=CARTESIAN_POINT('Ctrl Pts',(0.606419780073446,2.73140319464357,8.36663888888888));
#19110=CARTESIAN_POINT('Ctrl Pts',(-1.7871649975578,2.04969182184781,8.51418299899463));
#19111=CARTESIAN_POINT('Ctrl Pts',(-2.36693996130543,0.627621353124904,
8.60910673873));
#19112=CARTESIAN_POINT('Ctrl Pts',(-2.37260887298937,-0.00202072084187674,
8.65141010809499));
#19113=CARTESIAN_POINT('Ctrl Pts',(-2.37158591103805,-0.002113965830532,
7.84858989190503));
#19114=CARTESIAN_POINT('Ctrl Pts',(-2.37327853101496,-0.190408271679788,
7.86122670826915));
#19115=CARTESIAN_POINT('Ctrl Pts',(-2.26703071089283,-1.16154754141212,
7.92652848829996));
#19116=CARTESIAN_POINT('Ctrl Pts',(-0.9330321424437,-2.63859476601473,8.04449523199746));
#19117=CARTESIAN_POINT('Ctrl Pts',(1.70002224901497,-2.22320841823872,8.2024901229975));
#19118=CARTESIAN_POINT('Ctrl Pts',(2.79088864512093,0.208978201275766,8.36048501399757));
#19119=CARTESIAN_POINT('Ctrl Pts',(1.34997937336987,2.45158867054595,8.51847990499762));
#19120=CARTESIAN_POINT('Ctrl Pts',(-1.31557386100644,2.47022200101732,8.67647479599767));
#19121=CARTESIAN_POINT('Ctrl Pts',(-2.34084261733164,0.922522196646213,
8.78651145830014));
#19122=CARTESIAN_POINT('Ctrl Pts',(-2.37522208450983,0.0710785316625285,
8.84388315693593));
#19123=CARTESIAN_POINT('Ctrl Pts',(-2.3747901511292,0.00119133359606537,
8.84858989190503));
#19124=CARTESIAN_POINT('Origin',(0.,0.,-1.84858989190501));
#19125=CARTESIAN_POINT('',(-2.37396076251026,0.0016408096299993,6.65141010809499));
#19126=CARTESIAN_POINT('',(-2.36824488832617,0.00085307042009708,6.84858989190503));
#19127=CARTESIAN_POINT('',(-2.37175,-2.62313128856983E-13,-1.84858989190501));
#19128=CARTESIAN_POINT('Ctrl Pts',(-2.37396076251026,0.00164080962999946,
6.65141010809499));
#19129=CARTESIAN_POINT('Ctrl Pts',(-2.36860111288507,-0.675161988858878,
6.69694933132258));
#19130=CARTESIAN_POINT('Ctrl Pts',(-1.71220786555833,-2.14309654094568,
6.79510892492056));
#19131=CARTESIAN_POINT('Ctrl Pts',(0.771789132562049,-2.68935864031417,
6.94588888888888));
#19132=CARTESIAN_POINT('Ctrl Pts',(2.67339522049833,-0.825388609316905,
7.10375));
#19133=CARTESIAN_POINT('Ctrl Pts',(2.15357369271338,1.7861771220756,7.26161111111111));
#19134=CARTESIAN_POINT('Ctrl Pts',(-0.3168471224657,2.77991299546561,7.41947222222222));
#19135=CARTESIAN_POINT('Ctrl Pts',(-2.11399942046796,1.52539245310181,7.54940522121685));
#19136=CARTESIAN_POINT('Ctrl Pts',(-2.36856127073871,0.369714310321545,
7.62671784984111));
#19137=CARTESIAN_POINT('Ctrl Pts',(-2.36801892187683,0.000385579322849869,
7.65141010809499));
#19138=CARTESIAN_POINT('Ctrl Pts',(-2.36824488832617,0.000853070420097184,
6.84858989190503));
#19139=CARTESIAN_POINT('Ctrl Pts',(-2.36678180876479,-0.447463537758943,
6.87857025960238));
#19140=CARTESIAN_POINT('Ctrl Pts',(-2.02943011823198,-1.68535627820218,
6.96121559096642));
#19141=CARTESIAN_POINT('Ctrl Pts',(-0.0362940343214689,-2.79846637663312,
7.09652588599712));
#19142=CARTESIAN_POINT('Ctrl Pts',(2.32391314315961,-1.55953807940794,7.2545207769972));
#19143=CARTESIAN_POINT('Ctrl Pts',(2.57596499873257,1.09413693995685,7.41251566799723));
#19144=CARTESIAN_POINT('Ctrl Pts',(0.491210792034311,2.75525738831465,7.5705105589973));
#19145=CARTESIAN_POINT('Ctrl Pts',(-1.83676464589149,1.98397717256952,7.71586863363322));
#19146=CARTESIAN_POINT('Ctrl Pts',(-2.36622439910258,0.594323617306658,
7.80856174460247));
#19147=CARTESIAN_POINT('Ctrl Pts',(-2.37158591103805,-0.002113965830532,
7.84858989190503));
#19148=CARTESIAN_POINT('Origin',(0.,0.,-1.84858989190501));
#19149=CARTESIAN_POINT('',(-2.37251499866524,-0.00203510706959473,5.65141010809499));
#19150=CARTESIAN_POINT('',(-2.37459246787895,0.00132584644941116,5.84858989190502));
#19151=CARTESIAN_POINT('',(-2.37175,-2.62313128856983E-13,-1.84858989190501));
#19152=CARTESIAN_POINT('Ctrl Pts',(-2.37251499866524,-0.00203510706959476,
5.65141010809499));
#19153=CARTESIAN_POINT('Ctrl Pts',(-2.37392982983489,-0.158778764602934,
5.66194007206332));
#19154=CARTESIAN_POINT('Ctrl Pts',(-2.28863365792017,-1.09727074999648,
5.72509040640203));
#19155=CARTESIAN_POINT('Ctrl Pts',(-1.03894725747156,-2.59786392206505,
5.84086111111111));
#19156=CARTESIAN_POINT('Ctrl Pts',(1.60611030100396,-2.29100808867664,5.99872222222222));
#19157=CARTESIAN_POINT('Ctrl Pts',(2.79643351757374,0.090928230838667,6.15658333333333));
#19158=CARTESIAN_POINT('Ctrl Pts',(1.45388718569001,2.39050630885174,6.31444444444444));
#19159=CARTESIAN_POINT('Ctrl Pts',(-1.20551740739643,2.52488339173069,6.47230555555556));
#19160=CARTESIAN_POINT('Ctrl Pts',(-2.3208356274226,0.99330351170231,6.58462744343907));
#19161=CARTESIAN_POINT('Ctrl Pts',(-2.37479416424485,0.106880641648857,
6.64432896095221));
#19162=CARTESIAN_POINT('Ctrl Pts',(-2.37396076251026,0.00164080962999946,
6.65141010809499));
#19163=CARTESIAN_POINT('Ctrl Pts',(-2.37459246787895,0.00132584644941126,
5.84858989190502));
#19164=CARTESIAN_POINT('Ctrl Pts',(-2.3698592307678,-0.701510136856058,
5.8959138109356));
#19165=CARTESIAN_POINT('Ctrl Pts',(-1.6684907359976,-2.19471791424095,5.99590269363287));
#19166=CARTESIAN_POINT('Ctrl Pts',(0.864288593995119,-2.66190468356086,
6.14855653999681));
#19167=CARTESIAN_POINT('Ctrl Pts',(2.70163876039796,-0.730670463607777,
6.30655143099686));
#19168=CARTESIAN_POINT('Ctrl Pts',(2.08817696449889,1.86339697407977,6.46454632199692));
#19169=CARTESIAN_POINT('Ctrl Pts',(-0.419590302218696,2.76706980330411,
6.62254121299697));
#19170=CARTESIAN_POINT('Ctrl Pts',(-2.14308835195883,1.46541542002878,6.75055573629967));
#19171=CARTESIAN_POINT('Ctrl Pts',(-2.36935192507288,0.340071095547311,
6.82590529593569));
#19172=CARTESIAN_POINT('Ctrl Pts',(-2.36824488832617,0.000853070420097184,
6.84858989190503));
#19173=CARTESIAN_POINT('Origin',(0.,0.,-1.84858989190501));
#19174=CARTESIAN_POINT('',(-2.36803551809634,0.000435659979227324,4.65141010809499));
#19175=CARTESIAN_POINT('',(-2.37186713520955,-0.00210673407030348,4.84858989190502));
#19176=CARTESIAN_POINT('',(-2.37175,-2.62313128856983E-13,-1.84858989190501));
#19177=CARTESIAN_POINT('Ctrl Pts',(-2.36803551809634,0.000435659979227676,
4.65141010809499));
#19178=CARTESIAN_POINT('Ctrl Pts',(-2.36733685507668,-0.420470574046625,
4.67955118317444));
#19179=CARTESIAN_POINT('Ctrl Pts',(-2.06020439223756,-1.62937224150312,
4.76031262862425));
#19180=CARTESIAN_POINT('Ctrl Pts',(-0.135586668767159,-2.79462423533096,
4.89369444444444));
#19181=CARTESIAN_POINT('Ctrl Pts',(2.2650598786042,-1.64250178316317,5.05155555555556));
#19182=CARTESIAN_POINT('Ctrl Pts',(2.61412853009539,0.997316594419356,5.20941666666666));
#19183=CARTESIAN_POINT('Ctrl Pts',(0.595450368366912,2.73381550588105,5.36727777777778));
#19184=CARTESIAN_POINT('Ctrl Pts',(-1.79192767962886,2.0434990191552,5.51460892492054));
#19185=CARTESIAN_POINT('Ctrl Pts',(-2.36685963088812,0.624501153297232,
5.60931970169295));
#19186=CARTESIAN_POINT('Ctrl Pts',(-2.37251499866524,-0.00203510706959476,
5.65141010809499));
#19187=CARTESIAN_POINT('Ctrl Pts',(-2.37186713520955,-0.00210673407030307,
4.84858989190502));
#19188=CARTESIAN_POINT('Ctrl Pts',(-2.37348726775032,-0.180895246540068,
4.86059239860214));
#19189=CARTESIAN_POINT('Ctrl Pts',(-2.27367886126175,-1.14238681798702,
4.92525986896595));
#19190=CARTESIAN_POINT('Ctrl Pts',(-0.964512940920624,-2.62725067416123,
5.04259230299644));
#19191=CARTESIAN_POINT('Ctrl Pts',(1.67331967629405,-2.24337526486265,5.20058719399648));
#19192=CARTESIAN_POINT('Ctrl Pts',(2.79318773824162,0.175594923072764,5.35858208499656));
#19193=CARTESIAN_POINT('Ctrl Pts',(1.37919449268132,2.43527285317938,5.51657697599659));
#19194=CARTESIAN_POINT('Ctrl Pts',(-1.28594543116668,2.48577466117395,5.67457186699666));
#19195=CARTESIAN_POINT('Ctrl Pts',(-2.33566190719347,0.94159330950118,5.78524283896613));
#19196=CARTESIAN_POINT('Ctrl Pts',(-2.37512666773395,0.0806489125773547,
5.84324884726892));
#19197=CARTESIAN_POINT('Ctrl Pts',(-2.37459246787895,0.00132584644941126,
5.84858989190502));
#19198=CARTESIAN_POINT('Origin',(0.,0.,-1.84858989190501));
#19199=CARTESIAN_POINT('',(-2.37404189208837,0.00160568163382189,3.65141010809499));
#19200=CARTESIAN_POINT('',(-2.36815046112586,0.00071106261527204,3.84858989190502));
#19201=CARTESIAN_POINT('',(-2.37175,-2.62313128856983E-13,-1.84858989190501));
#19202=CARTESIAN_POINT('Ctrl Pts',(-2.37404189208837,0.0016056816338219,
3.65141010809499));
#19203=CARTESIAN_POINT('Ctrl Pts',(-2.36874097406567,-0.678301390146093,
3.69716229428555));
#19204=CARTESIAN_POINT('Ctrl Pts',(-1.70710264047504,-2.14919504149034,
3.79553485084648));
#19205=CARTESIAN_POINT('Ctrl Pts',(0.782578662553965,-2.68623882063674,
3.94652777777777));
#19206=CARTESIAN_POINT('Ctrl Pts',(2.67668699402767,-0.814650291328897,
4.10438888888889));
#19207=CARTESIAN_POINT('Ctrl Pts',(2.14638618582228,1.79480770611467,4.26225));
#19208=CARTESIAN_POINT('Ctrl Pts',(-0.328003825581952,2.77861869501174,
4.42011111111111));
#19209=CARTESIAN_POINT('Ctrl Pts',(-2.1171683957745,1.51896204170615,4.54983114714277));
#19210=CARTESIAN_POINT('Ctrl Pts',(-2.3686432695173,0.366572631058683,4.62693081280407));
#19211=CARTESIAN_POINT('Ctrl Pts',(-2.36803551809634,0.000435659979227676,
4.65141010809499));
#19212=CARTESIAN_POINT('Ctrl Pts',(-2.36815046112586,0.000711062615271901,
3.84858989190502));
#19213=CARTESIAN_POINT('Ctrl Pts',(-2.36695951468436,-0.438164069114789,
3.87793594993537));
#19214=CARTESIAN_POINT('Ctrl Pts',(-2.04015506879268,-1.66630099353556,
3.9599469716324));
#19215=CARTESIAN_POINT('Ctrl Pts',(-0.0697503817448946,-2.79783241149437,
4.09462295699612));
#19216=CARTESIAN_POINT('Ctrl Pts',(2.30510093209087,-1.58721170953314,4.25261784799616));
#19217=CARTESIAN_POINT('Ctrl Pts',(2.5888625630092,1.06326005653742,4.41061273899623));
#19218=CARTESIAN_POINT('Ctrl Pts',(0.524118009051023,2.74918744918107,4.56860762999628));
#19219=CARTESIAN_POINT('Ctrl Pts',(-1.82311086019465,2.00255204277458,4.71460001429921));
#19220=CARTESIAN_POINT('Ctrl Pts',(-2.36637840094874,0.603598422228309,
4.80792743493546));
#19221=CARTESIAN_POINT('Ctrl Pts',(-2.37186713520955,-0.00210673407030307,
4.84858989190502));
#19222=CARTESIAN_POINT('Origin',(0.,0.,-1.84858989190501));
#19223=CARTESIAN_POINT('',(-2.37242086931256,-0.00204814969984112,2.65141010809499));
#19224=CARTESIAN_POINT('',(-2.37437841508221,0.00145143062880153,2.84858989190502));
#19225=CARTESIAN_POINT('',(-2.37175,-2.62313128856983E-13,-1.84858989190501));
#19226=CARTESIAN_POINT('Ctrl Pts',(-2.37242086931256,-0.00204814969984169,
2.65141010809499));
#19227=CARTESIAN_POINT('Ctrl Pts',(-2.37386724785776,-0.161978223542019,
2.66215303502629));
#19228=CARTESIAN_POINT('Ctrl Pts',(-2.28652040521148,-1.10369798895945,
2.72551633232796));
#19229=CARTESIAN_POINT('Ctrl Pts',(-1.02851040967351,-2.60201352259292,
2.84149999999999));
#19230=CARTESIAN_POINT('Ctrl Pts',(1.61529402596567,-2.28454233775194,2.99936111111111));
#19231=CARTESIAN_POINT('Ctrl Pts',(2.79604598097933,0.102153087721166,3.15722222222222));
#19232=CARTESIAN_POINT('Ctrl Pts',(1.44427938842878,2.39632330140064,3.31508333333333));
#19233=CARTESIAN_POINT('Ctrl Pts',(-1.21564319790733,2.5200238088076,3.47294444444445));
#19234=CARTESIAN_POINT('Ctrl Pts',(-2.32270131739363,0.986891451715146,
3.58505336936499));
#19235=CARTESIAN_POINT('Ctrl Pts',(-2.37483765037521,0.103671339757588,
3.64454192391517));
#19236=CARTESIAN_POINT('Ctrl Pts',(-2.37404189208837,0.0016056816338219,
3.65141010809499));
#19237=CARTESIAN_POINT('Ctrl Pts',(-2.37437841508221,0.00145143062880148,
2.84858989190502));
#19238=CARTESIAN_POINT('Ctrl Pts',(-2.36936657242201,-0.69212851464997,
2.89527950126859));
#19239=CARTESIAN_POINT('Ctrl Pts',(-1.68411161328175,-2.17667922631145,
2.99463407429885));
#19240=CARTESIAN_POINT('Ctrl Pts',(0.832400628534772,-2.67204800324426,
3.1466536109958));
#19241=CARTESIAN_POINT('Ctrl Pts',(2.69270963387839,-0.762919488957052,
3.30464850199585));
#19242=CARTESIAN_POINT('Ctrl Pts',(2.11030679852043,1.83829718168443,3.4626433929959));
#19243=CARTESIAN_POINT('Ctrl Pts',(-0.386476751895552,2.77188871376435,
3.62063828399595));
#19244=CARTESIAN_POINT('Ctrl Pts',(-2.13403081733917,1.48458669705641,3.74928711696566));
#19245=CARTESIAN_POINT('Ctrl Pts',(-2.36909680859298,0.349449137499666,
3.82527098626868));
#19246=CARTESIAN_POINT('Ctrl Pts',(-2.36815046112586,0.000711062615271901,
3.84858989190502));
#19247=CARTESIAN_POINT('Origin',(0.,0.,-1.84858989190501));
#19248=CARTESIAN_POINT('',(-2.36805372255214,0.000487775483918624,1.65141010809499));
#19249=CARTESIAN_POINT('',(-2.37214954248261,-0.00208751672060303,1.84858989190502));
#19250=CARTESIAN_POINT('',(-2.37175,-2.62313128856983E-13,-1.84858989190501));
#19251=CARTESIAN_POINT('Ctrl Pts',(-2.36805372255214,0.000487775483918769,
1.65141010809499));
#19252=CARTESIAN_POINT('Ctrl Pts',(-2.36726911244657,-0.423596588857836,
1.6797641461374));
#19253=CARTESIAN_POINT('Ctrl Pts',(-2.0567282222087,-1.63578530702029,1.76073855455018));
#19254=CARTESIAN_POINT('Ctrl Pts',(-0.124366744542119,-2.79514315034066,
1.89433333333333));
#19255=CARTESIAN_POINT('Ctrl Pts',(2.27163476293377,-1.63339753074864,2.05219444444444));
#19256=CARTESIAN_POINT('Ctrl Pts',(2.61010413592219,1.00780309522069,2.21005555555555));
#19257=CARTESIAN_POINT('Ctrl Pts',(0.584471286669745,2.73618335546233,2.36791666666667));
#19258=CARTESIAN_POINT('Ctrl Pts',(-1.79666946585791,2.03730116384381,2.51503485084647));
#19259=CARTESIAN_POINT('Ctrl Pts',(-2.36678268187025,0.621381820955435,
2.60953266465592));
#19260=CARTESIAN_POINT('Ctrl Pts',(-2.37242086931256,-0.00204814969984169,
2.65141010809499));
#19261=CARTESIAN_POINT('Ctrl Pts',(-2.37214954248261,-0.00208751672060286,
1.84858989190502));
#19262=CARTESIAN_POINT('Ctrl Pts',(-2.37368814589582,-0.171375740131997,
1.85995808893514));
#19263=CARTESIAN_POINT('Ctrl Pts',(-2.28019409230745,-1.12323247312203,
1.92399124963194));
#19264=CARTESIAN_POINT('Ctrl Pts',(-0.995855715555496,-2.61553061219188,
2.04068937399542));
#19265=CARTESIAN_POINT('Ctrl Pts',(1.64637781974439,-2.26322161422709,2.19868426499547));
#19266=CARTESIAN_POINT('Ctrl Pts',(2.79508756969503,0.142186649832604,2.35667915599553));
#19267=CARTESIAN_POINT('Ctrl Pts',(1.40821242874264,2.41860884498944,2.51467404699558));
#19268=CARTESIAN_POINT('Ctrl Pts',(-1.25613315819632,2.50097199645567,2.67266893799564));
#19269=CARTESIAN_POINT('Ctrl Pts',(-2.33035893824447,0.960673681793537,
2.78397421963211));
#19270=CARTESIAN_POINT('Ctrl Pts',(-2.37501983264844,0.0902160608552179,
2.84261453760191));
#19271=CARTESIAN_POINT('Ctrl Pts',(-2.37437841508221,0.00145143062880148,
2.84858989190502));
#19272=CARTESIAN_POINT('Origin',(0.,0.,-1.84858989190501));
#19273=CARTESIAN_POINT('',(-2.37409249406917,0.00172857025301859,0.651410108094985));
#19274=CARTESIAN_POINT('',(-2.36806791026422,0.000580996437929415,0.848589891905023));
#19275=CARTESIAN_POINT('',(-2.37175,-2.62313128856983E-13,-1.84858989190501));
#19276=CARTESIAN_POINT('Ctrl Pts',(-2.37409249406917,0.00172857025301858,
0.651410108094986));
#19277=CARTESIAN_POINT('Ctrl Pts',(-2.36885059157359,-0.681255271864669,
0.697375257248508));
#19278=CARTESIAN_POINT('Ctrl Pts',(-1.70202128243095,-2.15553453151225,
0.7959607767724));
#19279=CARTESIAN_POINT('Ctrl Pts',(0.793380919254056,-2.68293732976497,
0.947166666666663));
#19280=CARTESIAN_POINT('Ctrl Pts',(2.67992237177449,-0.803971281251394,
1.10502777777777));
#19281=CARTESIAN_POINT('Ctrl Pts',(2.13917103413275,1.80344728451176,1.26288888888888));
#19282=CARTESIAN_POINT('Ctrl Pts',(-0.339158877291603,2.77725977180218,
1.42075));
#19283=CARTESIAN_POINT('Ctrl Pts',(-2.12031894951391,1.51253569372851,1.5502570730687));
#19284=CARTESIAN_POINT('Ctrl Pts',(-2.36872521807391,0.363433332120877,
1.62714377576703));
#19285=CARTESIAN_POINT('Ctrl Pts',(-2.36805372255214,0.000487775483918769,
1.65141010809499));
#19286=CARTESIAN_POINT('Ctrl Pts',(-2.36806791026422,0.000580996437929554,
0.848589891905023));
#19287=CARTESIAN_POINT('Ctrl Pts',(-2.36714590954407,-0.428850691797627,
0.877301640268363));
#19288=CARTESIAN_POINT('Ctrl Pts',(-2.05072593975983,-1.64725737587436,
0.958678352298389));
#19289=CARTESIAN_POINT('Ctrl Pts',(-0.103189861818606,-2.79677945469355,
1.0927200279951));
#19290=CARTESIAN_POINT('Ctrl Pts',(2.28595558559378,-1.6146683983646,1.25071491899515));
#19291=CARTESIAN_POINT('Ctrl Pts',(2.60139192527736,1.0322363870214,1.4087098099952));
#19292=CARTESIAN_POINT('Ctrl Pts',(0.556949311928898,2.7427217714679,1.56670470099526));
#19293=CARTESIAN_POINT('Ctrl Pts',(-1.80927361374524,2.02108563130788,1.7133313949652));
#19294=CARTESIAN_POINT('Ctrl Pts',(-2.36656032319539,0.612878624174093,
1.80729312526845));
#19295=CARTESIAN_POINT('Ctrl Pts',(-2.37214954248261,-0.00208751672060286,
1.84858989190502));
#19296=CARTESIAN_POINT('Origin',(0.,0.,15.5));
#19297=CARTESIAN_POINT('',(-2.86987326377042,0.00104132824445593,15.1339652973708));
#19298=CARTESIAN_POINT('Ctrl Pts',(-0.439445221994174,2.33068358199188,
15.62825));
#19299=CARTESIAN_POINT('Ctrl Pts',(-0.359491362851287,2.34930954683752,
15.6247606402091));
#19300=CARTESIAN_POINT('Ctrl Pts',(-0.27873128971825,2.36341107797762,15.6212855109979));
#19301=CARTESIAN_POINT('Ctrl Pts',(-0.197490043658781,2.37317361481181,
15.6178198845782));
#19302=CARTESIAN_POINT('Ctrl Pts',(-0.114097433923979,2.38319467509491,
15.6142624842978));
#19303=CARTESIAN_POINT('Ctrl Pts',(-0.0301970746788968,2.38864392614809,
15.610715096763));
#19304=CARTESIAN_POINT('Ctrl Pts',(0.0538748377108959,2.38966967391038,
15.6071726085593));
#19305=CARTESIAN_POINT('Ctrl Pts',(0.0936167287327529,2.39015455827456,
15.6054980281181));
#19306=CARTESIAN_POINT('Ctrl Pts',(0.133397101437596,2.38965022998153,15.6038245424699));
#19307=CARTESIAN_POINT('Ctrl Pts',(0.17318082101162,2.38816842541213,15.6021516114778));
#19308=CARTESIAN_POINT('Ctrl Pts',(0.19744268730314,2.38726475565179,15.601131384398));
#19309=CARTESIAN_POINT('Ctrl Pts',(0.221705799792773,2.38599750448324,15.6001113636003));
#19310=CARTESIAN_POINT('Ctrl Pts',(0.245962166148401,2.38436888753973,15.5990914265778));
#19311=CARTESIAN_POINT('Ctrl Pts',(0.26185491634123,2.38330181913124,15.5984231647255));
#19312=CARTESIAN_POINT('Ctrl Pts',(0.277745619245824,2.38207945021967,15.597754902985));
#19313=CARTESIAN_POINT('Ctrl Pts',(0.293615508622687,2.38070402970992,15.5970873017022));
#19314=CARTESIAN_POINT('Ctrl Pts',(0.379355905904818,2.37327303267301,15.5934804461119));
#19315=CARTESIAN_POINT('Ctrl Pts',(0.46460122999168,2.36137220783444,15.5898881158652));
#19316=CARTESIAN_POINT('Ctrl Pts',(0.548999070996607,2.3451645872232,15.5863050764217));
#19317=CARTESIAN_POINT('Ctrl Pts',(0.634137600151781,2.32881472609505,15.582690591685));
#19318=CARTESIAN_POINT('Ctrl Pts',(0.718414656351904,2.30808199543454,15.5790855615419));
#19319=CARTESIAN_POINT('Ctrl Pts',(0.801467682213623,2.28308069981211,15.5754846124216));
#19320=CARTESIAN_POINT('Ctrl Pts',(0.852459500288906,2.26773072905791,15.573273748452));
#19321=CARTESIAN_POINT('Ctrl Pts',(0.902989840792886,2.2507706713731,15.5710644228464));
#19322=CARTESIAN_POINT('Ctrl Pts',(0.952972256247749,2.23221757070223,15.5688553919549));
#19323=CARTESIAN_POINT('Ctrl Pts',(0.964785636442244,2.22783253188374,15.5683332858993));
#19324=CARTESIAN_POINT('Ctrl Pts',(0.976567164733754,2.22335887755768,15.5678112499871));
#19325=CARTESIAN_POINT('Ctrl Pts',(0.98830665315667,2.21880049805757,15.5672896716409));
#19326=CARTESIAN_POINT('Ctrl Pts',(1.07009362440554,2.18704306198486,15.5636559261431));
#19327=CARTESIAN_POINT('Ctrl Pts',(1.14996182974845,2.15113305037133,15.5600390318413));
#19328=CARTESIAN_POINT('Ctrl Pts',(1.22755227573139,2.11121890826833,15.5564336755567));
#19329=CARTESIAN_POINT('Ctrl Pts',(1.30476387614222,2.07149965222131,15.552845922899));
#19330=CARTESIAN_POINT('Ctrl Pts',(1.37972085381243,2.02781498993708,15.5492695958616));
#19331=CARTESIAN_POINT('Ctrl Pts',(1.45205674723287,1.98026157738062,15.5456994587133));
#19332=CARTESIAN_POINT('Ctrl Pts',(1.51163119176407,1.94109750537355,15.5427591627211));
#19333=CARTESIAN_POINT('Ctrl Pts',(1.56942781249227,1.89930836286272,15.5398230652386));
#19334=CARTESIAN_POINT('Ctrl Pts',(1.62522850219512,1.85492460083693,15.5368882414682));
#19335=CARTESIAN_POINT('Ctrl Pts',(1.65312884704655,1.83273271982404,15.5354208295831));
#19336=CARTESIAN_POINT('Ctrl Pts',(1.68052998038672,1.80989186082895,15.5339537361259));
#19337=CARTESIAN_POINT('Ctrl Pts',(1.70740302888556,1.78640394209333,15.532486595497));
#19338=CARTESIAN_POINT('Ctrl Pts',(1.72592667853778,1.77021366960761,15.5314752923321));
#19339=CARTESIAN_POINT('Ctrl Pts',(1.74419939199006,1.753715928893,15.5304639667541));
#19340=CARTESIAN_POINT('Ctrl Pts',(1.76221135665739,1.73691101229318,15.5294524990243));
#19341=CARTESIAN_POINT('Ctrl Pts',(1.77033011726031,1.72933631972932,15.528996587384));
#19342=CARTESIAN_POINT('Ctrl Pts',(1.77839409985328,1.72170084478485,15.5285407465195));
#19343=CARTESIAN_POINT('Ctrl Pts',(1.78639747681482,1.71400960641012,15.5280852527741));
#19344=CARTESIAN_POINT('Ctrl Pts',(1.84657495109044,1.65617910540199,15.5246603905846));
#19345=CARTESIAN_POINT('Ctrl Pts',(1.90341295390484,1.59512114682347,15.5212504095826));
#19346=CARTESIAN_POINT('Ctrl Pts',(1.95689046613085,1.53122773141625,15.5178508639384));
#19347=CARTESIAN_POINT('Ctrl Pts',(2.01194103421405,1.46545487347031,15.5143513197161));
#19348=CARTESIAN_POINT('Ctrl Pts',(2.06343093897923,1.39667671283205,15.5108628337987));
#19349=CARTESIAN_POINT('Ctrl Pts',(2.11130423046702,1.3252770563036,15.507380556377));
#19350=CARTESIAN_POINT('Ctrl Pts',(2.15745742078722,1.25644281002257,15.5040233981871));
#19351=CARTESIAN_POINT('Ctrl Pts',(2.20024928268006,1.18517117106803,15.500672010362));
#19352=CARTESIAN_POINT('Ctrl Pts',(2.23959635988792,1.11177753196584,15.4973220472993));
#19353=CARTESIAN_POINT('Ctrl Pts',(2.25681070616636,1.07966781485864,15.4958564384594));
#19354=CARTESIAN_POINT('Ctrl Pts',(2.27336525378777,1.04715163497876,15.4943911023279));
#19355=CARTESIAN_POINT('Ctrl Pts',(2.28925084670373,1.0142542353915,15.4929256750031));
#19356=CARTESIAN_POINT('Ctrl Pts',(2.29885484868501,0.994365352899876,15.4920397170785));
#19357=CARTESIAN_POINT('Ctrl Pts',(2.30821431569525,0.974337119524171,15.491153725822));
#19358=CARTESIAN_POINT('Ctrl Pts',(2.3173269757796,0.954175024263046,15.4902676208197));
#19359=CARTESIAN_POINT('Ctrl Pts',(2.32227232757467,0.943233251710468,15.4897867402729));
#19360=CARTESIAN_POINT('Ctrl Pts',(2.32714420559321,0.932253683866113,15.4893058986854));
#19361=CARTESIAN_POINT('Ctrl Pts',(2.33193873109372,0.921245710398884,15.4888254510349));
#19362=CARTESIAN_POINT('Ctrl Pts',(2.36754247444614,0.839501424730483,15.4852576871677));
#19363=CARTESIAN_POINT('Ctrl Pts',(2.39894281260828,0.756064329075142,15.4817059560376));
#19364=CARTESIAN_POINT('Ctrl Pts',(2.42608268559146,0.671340103595013,15.4781652340513));
#19365=CARTESIAN_POINT('Ctrl Pts',(2.453534139292,0.58564319725637,15.4745838626229));
#19366=CARTESIAN_POINT('Ctrl Pts',(2.47662715562456,0.498628540954889,15.4710137545713));
#19367=CARTESIAN_POINT('Ctrl Pts',(2.49525785992387,0.410687466692489,15.4674497112883));
#19368=CARTESIAN_POINT('Ctrl Pts',(2.51258257274376,0.328910963121187,15.4641355034428));
#19369=CARTESIAN_POINT('Ctrl Pts',(2.52604844140045,0.24633247953868,15.4608265399003));
#19370=CARTESIAN_POINT('Ctrl Pts',(2.53553303361489,0.163255416668028,15.4575186404574));
#19371=CARTESIAN_POINT('Ctrl Pts',(2.53942998139287,0.129121426694033,15.4561595191486));
#19372=CARTESIAN_POINT('Ctrl Pts',(2.54265436806282,0.0949032017028567,
15.4548005774761));
#19373=CARTESIAN_POINT('Ctrl Pts',(2.54519570834653,0.0606216731012661,
15.4534415254952));
#19374=CARTESIAN_POINT('Ctrl Pts',(2.54650804671318,0.0429188233335401,
15.4527397162695));
#19375=CARTESIAN_POINT('Ctrl Pts',(2.5476382209856,0.0251990932110098,15.4520378776284));
#19376=CARTESIAN_POINT('Ctrl Pts',(2.54858465973821,0.00746537430393359,
15.4513359696452));
#19377=CARTESIAN_POINT('Ctrl Pts',(2.54936740774304,-0.00720121986763361,
15.4507554597369));
#19378=CARTESIAN_POINT('Ctrl Pts',(2.55002444266908,-0.0218786230829287,
15.4501748534934));
#19379=CARTESIAN_POINT('Ctrl Pts',(2.55055443165925,-0.0365475000712079,
15.4495948274855));
#19380=CARTESIAN_POINT('Ctrl Pts',(2.55387898415761,-0.128563471239416,
15.4459563992365));
#19381=CARTESIAN_POINT('Ctrl Pts',(2.55221836548087,-0.22040066645441,15.4423345418383));
#19382=CARTESIAN_POINT('Ctrl Pts',(2.5454697064449,-0.311650010793409,15.4387239299593));
#19383=CARTESIAN_POINT('Ctrl Pts',(2.53872104740894,-0.402899355132408,
15.4351133180804));
#19384=CARTESIAN_POINT('Ctrl Pts',(2.52688470709894,-0.49356189746232,15.4315139517205));
#19385=CARTESIAN_POINT('Ctrl Pts',(2.50980235603637,-0.583236219097685,
15.4279205055482));
#19386=CARTESIAN_POINT('Ctrl Pts',(2.49326213150481,-0.670064631014266,
15.424441101202));
#19387=CARTESIAN_POINT('Ctrl Pts',(2.47180332144007,-0.755967381987536,
15.420967247239));
#19388=CARTESIAN_POINT('Ctrl Pts',(2.44569482135312,-0.840684658565203,
15.4174941094224));
#19389=CARTESIAN_POINT('Ctrl Pts',(2.43658807165331,-0.870234384917672,
15.4162826650015));
#19390=CARTESIAN_POINT('Ctrl Pts',(2.42691516765274,-0.899639766052948,
15.41507130771));
#19391=CARTESIAN_POINT('Ctrl Pts',(2.41668612527745,-0.928889320342703,
15.4138598323975));
#19392=CARTESIAN_POINT('Ctrl Pts',(2.41079789512425,-0.945726488595391,
15.4131624606198));
#19393=CARTESIAN_POINT('Ctrl Pts',(2.40472537046329,-0.962512016907764,
15.4124650497348));
#19394=CARTESIAN_POINT('Ctrl Pts',(2.39847036187175,-0.979243667871416,
15.4117675606113));
#19395=CARTESIAN_POINT('Ctrl Pts',(2.39421301098727,-0.990631743201221,
15.4112928281));
#19396=CARTESIAN_POINT('Ctrl Pts',(2.38987156242605,-1.0019935463669,15.4108181134517));
#19397=CARTESIAN_POINT('Ctrl Pts',(2.38545028303317,-1.01331939423191,15.4103437824454));
#19398=CARTESIAN_POINT('Ctrl Pts',(2.35279097735238,-1.09698167717045,15.4068399728119));
#19399=CARTESIAN_POINT('Ctrl Pts',(2.31572987674733,-1.17881857921774,15.4033514296728));
#19400=CARTESIAN_POINT('Ctrl Pts',(2.27459874133947,-1.25857844945699,15.3998733992833));
#19401=CARTESIAN_POINT('Ctrl Pts',(2.23281288372258,-1.33960793109688,15.396340005877));
#19402=CARTESIAN_POINT('Ctrl Pts',(2.18682594253521,-1.41849449977561,15.3928174625663));
#19403=CARTESIAN_POINT('Ctrl Pts',(2.13693151879332,-1.49496175096055,15.3893007849646));
#19404=CARTESIAN_POINT('Ctrl Pts',(2.08679723793274,-1.57179660263405,15.385767201663));
#19405=CARTESIAN_POINT('Ctrl Pts',(2.03271725897117,-1.64618961960946,15.3822395406022));
#19406=CARTESIAN_POINT('Ctrl Pts',(1.97494281786374,-1.71783598585985,15.3787127451654));
#19407=CARTESIAN_POINT('Ctrl Pts',(1.95216878512211,-1.74607817495815,15.3773225222016));
#19408=CARTESIAN_POINT('Ctrl Pts',(1.92882022676702,-1.77389324483966,15.3759324337425));
#19409=CARTESIAN_POINT('Ctrl Pts',(1.90491084697345,-1.80126106485015,15.3745421700657));
#19410=CARTESIAN_POINT('Ctrl Pts',(1.89303589564547,-1.8148537022746,15.3738516748025));
#19411=CARTESIAN_POINT('Ctrl Pts',(1.88102258946071,-1.82833599951471,15.3731611363172));
#19412=CARTESIAN_POINT('Ctrl Pts',(1.86887253021617,-1.84170540057035,15.3724705166642));
#19413=CARTESIAN_POINT('Ctrl Pts',(1.86055716973053,-1.85085526453538,15.3719978645349));
#19414=CARTESIAN_POINT('Ctrl Pts',(1.8521789913077,-1.85995082597714,15.3715252464369));
#19415=CARTESIAN_POINT('Ctrl Pts',(1.84374494253208,-1.86898463564396,15.3710530027583));
#19416=CARTESIAN_POINT('Ctrl Pts',(1.77862481272331,-1.93873557897155,15.3674067623267));
#19417=CARTESIAN_POINT('Ctrl Pts',(1.71007452953627,-2.00492197279666,15.3637769310107));
#19418=CARTESIAN_POINT('Ctrl Pts',(1.63841756617314,-2.06724394639147,15.3601581531957));
#19419=CARTESIAN_POINT('Ctrl Pts',(1.56864469297252,-2.1279272764847,15.3566345245939));
#19420=CARTESIAN_POINT('Ctrl Pts',(1.49592552744324,-2.18494739655425,15.3531213758712));
#19421=CARTESIAN_POINT('Ctrl Pts',(1.42051657448793,-2.237996979208,15.3496137628515));
#19422=CARTESIAN_POINT('Ctrl Pts',(1.34626553575621,-2.29023197866037,15.3461600096832));
#19423=CARTESIAN_POINT('Ctrl Pts',(1.26940602418092,-2.33861808827242,15.3427116235202));
#19424=CARTESIAN_POINT('Ctrl Pts',(1.19015227451303,-2.38282228508801,15.3392638844625));
#19425=CARTESIAN_POINT('Ctrl Pts',(1.16438136391748,-2.39719614637352,15.3381427845096));
#19426=CARTESIAN_POINT('Ctrl Pts',(1.1383570943619,-2.4111274748391,15.3370217529787));
#19427=CARTESIAN_POINT('Ctrl Pts',(1.11208629310672,-2.42460372067378,15.3359006275904));
#19428=CARTESIAN_POINT('Ctrl Pts',(1.09252404263768,-2.4346386523776,15.3350657944447));
#19429=CARTESIAN_POINT('Ctrl Pts',(1.07282508844486,-2.44442123549769,15.3342309092564));
#19430=CARTESIAN_POINT('Ctrl Pts',(1.05299217133848,-2.4539460706498,15.3333959050218));
#19431=CARTESIAN_POINT('Ctrl Pts',(1.04038456497523,-2.46000092237074,15.3328651003678));
#19432=CARTESIAN_POINT('Ctrl Pts',(1.02772285622574,-2.46595150778408,15.3323342505181));
#19433=CARTESIAN_POINT('Ctrl Pts',(1.01502087310116,-2.47179063085649,15.3318038822616));
#19434=CARTESIAN_POINT('Ctrl Pts',(0.982652722257195,-2.48667032440912,
15.3304523578927));
#19435=CARTESIAN_POINT('Ctrl Pts',(0.950002091670773,-2.50083650005249,
15.3291030741213));
#19436=CARTESIAN_POINT('Ctrl Pts',(0.917084170499721,-2.5142729570447,15.3277557583224));
#19437=CARTESIAN_POINT('Ctrl Pts',(0.834495683370104,-2.5479839757206,15.3243754484619));
#19438=CARTESIAN_POINT('Ctrl Pts',(0.750226663082229,-2.57710500546031,
15.3210075263739));
#19439=CARTESIAN_POINT('Ctrl Pts',(0.664646844355562,-2.60177034865307,
15.317647686521));
#19440=CARTESIAN_POINT('Ctrl Pts',(0.576787650214132,-2.6270926408521,15.3141983590239));
#19441=CARTESIAN_POINT('Ctrl Pts',(0.487546169865586,-2.64771888106776,
15.3107575500279));
#19442=CARTESIAN_POINT('Ctrl Pts',(0.397298853288816,-2.66374516605354,
15.3073206007236));
#19443=CARTESIAN_POINT('Ctrl Pts',(0.308910977458226,-2.67944124812091,
15.3039544657529));
#19444=CARTESIAN_POINT('Ctrl Pts',(0.219557440695963,-2.69072476824651,
15.3005920330634));
#19445=CARTESIAN_POINT('Ctrl Pts',(0.129581594551193,-2.69764046998944,
15.2972289259214));
#19446=CARTESIAN_POINT('Ctrl Pts',(0.0974227261046785,-2.7001122571645,
15.2960268953233));
#19447=CARTESIAN_POINT('Ctrl Pts',(0.0651843226484069,-2.70202565483482,
15.2948247785662));
#19448=CARTESIAN_POINT('Ctrl Pts',(0.0328820436324132,-2.7033813247538,
15.2936223758136));
#19449=CARTESIAN_POINT('Ctrl Pts',(0.0192199250543532,-2.70395469987624,
15.2931138244208));
#19450=CARTESIAN_POINT('Ctrl Pts',(0.00555605037576419,-2.70442788901379,
15.2926055817652));
#19451=CARTESIAN_POINT('Ctrl Pts',(-0.00810768527292701,-2.70480131817288,
15.2920976575977));
#19452=CARTESIAN_POINT('Ctrl Pts',(-0.102177189495074,-2.70737223265483,
15.2886007973064));
#19453=CARTESIAN_POINT('Ctrl Pts',(-0.196248953232544,-2.705219350857,15.2851186519246));
#19454=CARTESIAN_POINT('Ctrl Pts',(-0.28992790026966,-2.69846111693802,
15.2816464960614));
#19455=CARTESIAN_POINT('Ctrl Pts',(-0.384721183626751,-2.69162249200534,
15.2781330379685));
#19456=CARTESIAN_POINT('Ctrl Pts',(-0.479113197863739,-2.68006831395088,
15.2746298084638));
#19457=CARTESIAN_POINT('Ctrl Pts',(-0.572703609774366,-2.66386867615587,
15.2711319115131));
#19458=CARTESIAN_POINT('Ctrl Pts',(-0.670406973022026,-2.64695712438838,
15.2674802949704));
#19459=CARTESIAN_POINT('Ctrl Pts',(-0.767237930320469,-2.62498318167097,
15.2638344899723));
#19460=CARTESIAN_POINT('Ctrl Pts',(-0.862734200133818,-2.5979664405403,
15.2601889262148));
#19461=CARTESIAN_POINT('Ctrl Pts',(-0.899309423475345,-2.58761898568426,
15.258792669493));
#19462=CARTESIAN_POINT('Ctrl Pts',(-0.935688693950487,-2.57653116703875,
15.2573964481588));
#19463=CARTESIAN_POINT('Ctrl Pts',(-0.971845190453781,-2.56470173355219,
15.2559999492582));
#19464=CARTESIAN_POINT('Ctrl Pts',(-0.985718422450195,-2.56016278506391,
15.2554641132369));
#19465=CARTESIAN_POINT('Ctrl Pts',(-0.999558849945709,-2.55551463851664,
15.2549282363508));
#19466=CARTESIAN_POINT('Ctrl Pts',(-1.01336493152648,-2.55075717270086,
15.254392300921));
#19467=CARTESIAN_POINT('Ctrl Pts',(-1.02713823497804,-2.5460110019675,15.2538576378986));
#19468=CARTESIAN_POINT('Ctrl Pts',(-1.0408680078023,-2.54115923920241,15.2533232792799));
#19469=CARTESIAN_POINT('Ctrl Pts',(-1.05455083068562,-2.53620294641156,
15.2527892870021));
#19470=CARTESIAN_POINT('Ctrl Pts',(-1.14480706402235,-2.50350966941525,
15.2492669048126));
#19471=CARTESIAN_POINT('Ctrl Pts',(-1.23304972084596,-2.46626241239109,
15.2457593395817));
#19472=CARTESIAN_POINT('Ctrl Pts',(-1.3188786706842,-2.42453542284507,15.242261762893));
#19473=CARTESIAN_POINT('Ctrl Pts',(-1.40341018907482,-2.38343919842613,
15.238817057246));
#19474=CARTESIAN_POINT('Ctrl Pts',(-1.48560133565556,-2.33799743942912,
15.2353820404405));
#19475=CARTESIAN_POINT('Ctrl Pts',(-1.56505752288372,-2.28823266258407,
15.2319520997326));
#19476=CARTESIAN_POINT('Ctrl Pts',(-1.59875150777533,-2.26712954025155,
15.2304976079627));
#19477=CARTESIAN_POINT('Ctrl Pts',(-1.63195344745741,-2.24524844976825,
15.2290440290004));
#19478=CARTESIAN_POINT('Ctrl Pts',(-1.66463195977674,-2.22258855435451,
15.2275910110965));
#19479=CARTESIAN_POINT('Ctrl Pts',(-1.74176819837999,-2.16910083489293,
15.2241612241271));
#19480=CARTESIAN_POINT('Ctrl Pts',(-1.81599039866318,-2.11127647963352,
15.2207345632396));
#19481=CARTESIAN_POINT('Ctrl Pts',(-1.88715256813859,-2.04946422501414,
15.2173064022613));
#19482=CARTESIAN_POINT('Ctrl Pts',(-1.90164577925548,-2.03687526008497,
15.2166082074035));
#19483=CARTESIAN_POINT('Ctrl Pts',(-1.91601194648249,-2.02412075255685,
15.215909950323));
#19484=CARTESIAN_POINT('Ctrl Pts',(-1.9302496520377,-2.01120346334021,15.2152115919387));
#19485=CARTESIAN_POINT('Ctrl Pts',(-1.94128816753001,-2.0011886687103,15.2146701535858));
#19486=CARTESIAN_POINT('Ctrl Pts',(-1.95224352654855,-1.99108137253609,
15.2141289446068));
#19487=CARTESIAN_POINT('Ctrl Pts',(-1.96311133771197,-1.98088698275119,
15.2135881466736));
#19488=CARTESIAN_POINT('Ctrl Pts',(-2.03178675603926,-1.91646702066845,
15.2101707589647));
#19489=CARTESIAN_POINT('Ctrl Pts',(-2.09701995613675,-1.8485265277173,15.2067672577273));
#19490=CARTESIAN_POINT('Ctrl Pts',(-2.15871310631003,-1.77747212767664,
15.2033732357386));
#19491=CARTESIAN_POINT('Ctrl Pts',(-2.22164945390415,-1.7049858888237,15.1999108197811));
#19492=CARTESIAN_POINT('Ctrl Pts',(-2.28090217022322,-1.62925832538052,
15.19645826896));
#19493=CARTESIAN_POINT('Ctrl Pts',(-2.33633512040192,-1.55067589533689,
15.1930109042136));
#19494=CARTESIAN_POINT('Ctrl Pts',(-2.39218601791983,-1.47150097801918,
15.1895375474008));
#19495=CARTESIAN_POINT('Ctrl Pts',(-2.44415984798534,-1.38942718616138,
15.1860694551604));
#19496=CARTESIAN_POINT('Ctrl Pts',(-2.49207710040016,-1.30481547317471,
15.1826018417945));
#19497=CARTESIAN_POINT('Ctrl Pts',(-2.52022211747796,-1.25511733759765,
15.1805650798249));
#19498=CARTESIAN_POINT('Ctrl Pts',(-2.54696681998739,-1.20454303320315,
15.1785284830672));
#19499=CARTESIAN_POINT('Ctrl Pts',(-2.57226731600719,-1.15316195438398,
15.1764910817393));
#19500=CARTESIAN_POINT('Ctrl Pts',(-2.57933924906923,-1.13880004030214,
15.1759215922795));
#19501=CARTESIAN_POINT('Ctrl Pts',(-2.58629893239321,-1.12437358425022,
15.1753519825172));
#19502=CARTESIAN_POINT('Ctrl Pts',(-2.59313735551554,-1.10990147500019,
15.1747829112963));
#19503=CARTESIAN_POINT('Ctrl Pts',(-2.63517066423893,-1.02094666405867,
15.1712850367298));
#19504=CARTESIAN_POINT('Ctrl Pts',(-2.6726976453638,-0.930127060905838,
15.167801819036));
#19505=CARTESIAN_POINT('Ctrl Pts',(-2.70558302354023,-0.837840896222647,
15.1643285389057));
#19506=CARTESIAN_POINT('Ctrl Pts',(-2.73847376195491,-0.745539689114618,
15.1608546926391));
#19507=CARTESIAN_POINT('Ctrl Pts',(-2.76672184052432,-0.651770570287676,
15.1573907871758));
#19508=CARTESIAN_POINT('Ctrl Pts',(-2.79014819101862,-0.556903769359717,
15.1539321008988));
#19509=CARTESIAN_POINT('Ctrl Pts',(-2.81305355218475,-0.464146754627161,
15.1505503339286));
#19510=CARTESIAN_POINT('Ctrl Pts',(-2.83134952927604,-0.370339481518358,
15.1471735565822));
#19511=CARTESIAN_POINT('Ctrl Pts',(-2.8448219024633,-0.275813943398833,
15.1437973553073));
#19512=CARTESIAN_POINT('Ctrl Pts',(-2.85447686455589,-0.208072315799913,
15.1413778042102));
#19513=CARTESIAN_POINT('Ctrl Pts',(-2.86165354894421,-0.139961477196466,
15.1389585489751));
#19514=CARTESIAN_POINT('Ctrl Pts',(-2.86625656775569,-0.071602632167948,
15.1365379651471));
#19515=CARTESIAN_POINT('Ctrl Pts',(-2.8678889837078,-0.0473598311579388,
15.1356795285827));
#19516=CARTESIAN_POINT('Ctrl Pts',(-2.86919553394546,-0.0231160969724086,
15.1348219958471));
#19517=CARTESIAN_POINT('Ctrl Pts',(-2.87017396612668,0.00112290304428943,
15.1339652973708));
#19518=CARTESIAN_POINT('',(0.261080338132197,2.92584241055005,15.058));
#19519=CARTESIAN_POINT('Ctrl Pts',(0.260984867623723,2.92515103163649,15.058));
#19520=CARTESIAN_POINT('Ctrl Pts',(0.163110290089364,2.92129299518303,15.0703787026841));
#19521=CARTESIAN_POINT('Ctrl Pts',(0.0656985383021158,2.91278590387498,
15.0828015605825));
#19522=CARTESIAN_POINT('Ctrl Pts',(-0.0308724856851826,2.89964343902045,
15.0952881213498));
#19523=CARTESIAN_POINT('Ctrl Pts',(-0.13093434020212,2.88602590291106,15.1082260438789));
#19524=CARTESIAN_POINT('Ctrl Pts',(-0.230094798512676,2.86743186329655,
15.121232357953));
#19525=CARTESIAN_POINT('Ctrl Pts',(-0.327908726704405,2.84382209488468,
15.1343288085909));
#19526=CARTESIAN_POINT('Ctrl Pts',(-0.401269172848201,2.82611476857578,
15.1441511465694));
#19527=CARTESIAN_POINT('Ctrl Pts',(-0.473871776581697,2.80558493098147,
15.154024186365));
#19528=CARTESIAN_POINT('Ctrl Pts',(-0.54551386023679,2.78219703023119,15.1639571016578));
#19529=CARTESIAN_POINT('Ctrl Pts',(-0.599245422978111,2.76465610466849,
15.1714067881273));
#19530=CARTESIAN_POINT('Ctrl Pts',(-0.652436445713434,2.74550717996222,
15.178890154564));
#19531=CARTESIAN_POINT('Ctrl Pts',(-0.704995275147146,2.7247296345796,15.186411071114));
#19532=CARTESIAN_POINT('Ctrl Pts',(-0.720729468886594,2.71850959642421,
15.1886625588158));
#19533=CARTESIAN_POINT('Ctrl Pts',(-0.736406966678059,2.71214357207348,
15.1909174117022));
#19534=CARTESIAN_POINT('Ctrl Pts',(-0.752025204049111,2.70563092815761,
15.1931757336031));
#19535=CARTESIAN_POINT('Ctrl Pts',(-0.764775912501757,2.70031401422844,
15.1950194246335));
#19536=CARTESIAN_POINT('Ctrl Pts',(-0.777478081511626,2.69490314594757,
15.196864120682));
#19537=CARTESIAN_POINT('Ctrl Pts',(-0.790130440968904,2.6893983882733,15.1987098648068));
#19538=CARTESIAN_POINT('Ctrl Pts',(-0.873485337988913,2.65313254310755,
15.2108697952897));
#19539=CARTESIAN_POINT('Ctrl Pts',(-0.954683148186728,2.61279395749136,
15.2230755503321));
#19540=CARTESIAN_POINT('Ctrl Pts',(-1.0333900295422,2.56835839969231,15.2353460721376));
#19541=CARTESIAN_POINT('Ctrl Pts',(-1.07474974365993,2.54500793864519,15.2417941141031));
#19542=CARTESIAN_POINT('Ctrl Pts',(-1.11542111238663,2.52052546068703,15.2482600407761));
#19543=CARTESIAN_POINT('Ctrl Pts',(-1.15535178122673,2.49490314259947,15.2547466008415));
#19544=CARTESIAN_POINT('Ctrl Pts',(-1.23327915249916,2.44489947493076,15.2674055567063));
#19545=CARTESIAN_POINT('Ctrl Pts',(-1.30838829429154,2.39055588937394,15.2801430971848));
#19546=CARTESIAN_POINT('Ctrl Pts',(-1.38046450469962,2.33219918561456,15.2929796526032));
#19547=CARTESIAN_POINT('Ctrl Pts',(-1.45426350057602,2.27244762382022,15.3061230309111));
#19548=CARTESIAN_POINT('Ctrl Pts',(-1.52488347180723,2.20848778279982,15.3193702140928));
#19549=CARTESIAN_POINT('Ctrl Pts',(-1.59204074405781,2.14065188994946,15.332743132764));
#19550=CARTESIAN_POINT('Ctrl Pts',(-1.60237109058904,2.13021715582588,15.3348001979094));
#19551=CARTESIAN_POINT('Ctrl Pts',(-1.61262065491134,2.1196893711682,15.3368604944486));
#19552=CARTESIAN_POINT('Ctrl Pts',(-1.62278430900332,2.10907388768773,15.3389232952054));
#19553=CARTESIAN_POINT('Ctrl Pts',(-1.68486768809848,2.04423056665054,15.3515236493914));
#19554=CARTESIAN_POINT('Ctrl Pts',(-1.74353795945352,1.97633977637267,15.3641743680265));
#19555=CARTESIAN_POINT('Ctrl Pts',(-1.79863355499942,1.90572574364455,15.3768970731667));
#19556=CARTESIAN_POINT('Ctrl Pts',(-1.8536060338742,1.83526950510231,15.3895913481376));
#19557=CARTESIAN_POINT('Ctrl Pts',(-1.90502010402237,1.76210117952091,15.4023572882508));
#19558=CARTESIAN_POINT('Ctrl Pts',(-1.95266740197694,1.68652354076833,15.4152163709358));
#19559=CARTESIAN_POINT('Ctrl Pts',(-1.999553014057,1.61215408007279,15.4278698893587));
#19560=CARTESIAN_POINT('Ctrl Pts',(-2.04279147033365,1.53545080587127,15.4406135962167));
#19561=CARTESIAN_POINT('Ctrl Pts',(-2.08213462636226,1.45669772176484,15.4534679553077));
#19562=CARTESIAN_POINT('Ctrl Pts',(-2.10370638024081,1.41351760306046,15.4605159681915));
#19563=CARTESIAN_POINT('Ctrl Pts',(-2.12410620181193,1.36972125073741,15.4675972464718));
#19564=CARTESIAN_POINT('Ctrl Pts',(-2.14328646703913,1.32535636167276,15.4747151632939));
#19565=CARTESIAN_POINT('Ctrl Pts',(-2.15012579550102,1.30953666132481,15.4772532810172));
#19566=CARTESIAN_POINT('Ctrl Pts',(-2.15681001155505,1.29364468163272,15.4797960573454));
#19567=CARTESIAN_POINT('Ctrl Pts',(-2.16333680365848,1.27768262506038,15.4823436452153));
#19568=CARTESIAN_POINT('Ctrl Pts',(-2.16791412260327,1.2664882400105,15.4841302996752));
#19569=CARTESIAN_POINT('Ctrl Pts',(-2.17241292255598,1.25526195256421,15.4859189101699));
#19570=CARTESIAN_POINT('Ctrl Pts',(-2.17682958710993,1.24401228867859,15.4877083034276));
#19571=CARTESIAN_POINT('Ctrl Pts',(-2.20791015801245,1.16484712416239,15.5003004673422));
#19572=CARTESIAN_POINT('Ctrl Pts',(-2.2349734122897,1.08441291813616,15.5129492481641));
#19573=CARTESIAN_POINT('Ctrl Pts',(-2.25783961089921,1.00297802743715,15.5256767231474));
#19574=CARTESIAN_POINT('Ctrl Pts',(-2.28035828534265,0.922780797311416,
15.5382107639178));
#19575=CARTESIAN_POINT('Ctrl Pts',(-2.29880657051476,0.841612257746407,
15.5508211250137));
#19576=CARTESIAN_POINT('Ctrl Pts',(-2.31296316132111,0.759731453145844,
15.5635288923091));
#19577=CARTESIAN_POINT('Ctrl Pts',(-2.32670958827523,0.680223009708963,
15.5758684730222));
#19578=CARTESIAN_POINT('Ctrl Pts',(-2.33640931253598,0.600042348520933,
15.5882998973352));
#19579=CARTESIAN_POINT('Ctrl Pts',(-2.34181299591968,0.519439649300842,
15.6008424709262));
#19580=CARTESIAN_POINT('Ctrl Pts',(-2.34572284670801,0.461119332452094,
15.609917686434));
#19581=CARTESIAN_POINT('Ctrl Pts',(-2.34738263953658,0.402578305857885,
15.6190510917899));
#19582=CARTESIAN_POINT('Ctrl Pts',(-2.34668236863854,0.343918483395394,
15.62825));
#19583=CARTESIAN_POINT('',(-2.14373220034752,2.0119373894844,15.058));
#19584=CARTESIAN_POINT('Origin',(0.,0.,15.058));
#19585=CARTESIAN_POINT('Ctrl Pts',(-2.87017396612668,0.00112290304428943,
15.1339652973708));
#19586=CARTESIAN_POINT('Ctrl Pts',(-2.87266912500978,0.0629362380616879,
15.1317805789463));
#19587=CARTESIAN_POINT('Ctrl Pts',(-2.87303098230106,0.124718621761705,
15.1296012856735));
#19588=CARTESIAN_POINT('Ctrl Pts',(-2.87121685856479,0.18637804904607,15.1274262638706));
#19589=CARTESIAN_POINT('Ctrl Pts',(-2.86841400163638,0.281643079490827,
15.1240658123162));
#19590=CARTESIAN_POINT('Ctrl Pts',(-2.86041988710444,0.376614623554742,
15.1207155571276));
#19591=CARTESIAN_POINT('Ctrl Pts',(-2.84750858059062,0.47099184224787,15.1173712434175));
#19592=CARTESIAN_POINT('Ctrl Pts',(-2.83433033308302,0.567320307975548,
15.1139577860911));
#19593=CARTESIAN_POINT('Ctrl Pts',(-2.81602924148459,0.663030385704492,
15.1105505184628));
#19594=CARTESIAN_POINT('Ctrl Pts',(-2.79284156103339,0.757800921120369,
15.1071449162423));
#19595=CARTESIAN_POINT('Ctrl Pts',(-2.77879319434313,0.815218101582043,
15.1050816159094));
#19596=CARTESIAN_POINT('Ctrl Pts',(-2.76295010551778,0.872290339259573,
15.1030189268812));
#19597=CARTESIAN_POINT('Ctrl Pts',(-2.74535586092349,0.928944130664371,
15.100955843023));
#19598=CARTESIAN_POINT('Ctrl Pts',(-2.7354097693855,0.960970728468381,15.099789574088));
#19599=CARTESIAN_POINT('Ctrl Pts',(-2.72490394590206,0.992863566804536,
15.098623178978));
#19600=CARTESIAN_POINT('Ctrl Pts',(-2.7138453785436,1.0246089965303,15.0974564759315));
#19601=CARTESIAN_POINT('Ctrl Pts',(-2.70868377697821,1.03942621963478,15.0969119156755));
#19602=CARTESIAN_POINT('Ctrl Pts',(-2.7034040983514,1.05420445638712,15.0963675402945));
#19603=CARTESIAN_POINT('Ctrl Pts',(-2.69801003661965,1.06893536837389,15.0958235919881));
#19604=CARTESIAN_POINT('Ctrl Pts',(-2.66394262772994,1.16197175299988,15.0923881642358));
#19605=CARTESIAN_POINT('Ctrl Pts',(-2.62528653689294,1.25320878716493,15.0889665364856));
#19606=CARTESIAN_POINT('Ctrl Pts',(-2.58232115247044,1.34232723597939,15.0855542358814));
#19607=CARTESIAN_POINT('Ctrl Pts',(-2.53887733631532,1.43243804397901,15.0821039383428));
#19608=CARTESIAN_POINT('Ctrl Pts',(-2.49102735184572,1.52038366982231,15.0786631768276));
#19609=CARTESIAN_POINT('Ctrl Pts',(-2.43900735397324,1.60582293428401,15.0752273273902));
#19610=CARTESIAN_POINT('Ctrl Pts',(-2.38725398360023,1.69082428143753,15.071809088333));
#19611=CARTESIAN_POINT('Ctrl Pts',(-2.33137274895099,1.77334571203064,15.0683957111292));
#19612=CARTESIAN_POINT('Ctrl Pts',(-2.27155099682431,1.8530278346518,15.064982642569));
#19613=CARTESIAN_POINT('Ctrl Pts',(-2.23076137590659,1.90735930205439,15.0626554326866));
#19614=CARTESIAN_POINT('Ctrl Pts',(-2.18813878650124,1.96037022431859,15.0603283662998));
#19615=CARTESIAN_POINT('Ctrl Pts',(-2.14373220034752,2.0119373894844,15.058));
#19616=CARTESIAN_POINT('',(-2.,-2.44929359829471E-16,16.));
#19617=CARTESIAN_POINT('',(-2.5,-3.06161699786838E-16,15.5));
#19618=CARTESIAN_POINT('Origin',(0.,0.,16.));
#19619=CARTESIAN_POINT('Ctrl Pts',(1.70810875200393,-2.39535560853239,-0.329233991005387));
#19620=CARTESIAN_POINT('Ctrl Pts',(2.5000696979919,-1.83061464970825,-0.276613620635017));
#19621=CARTESIAN_POINT('Ctrl Pts',(3.46698259537958,0.135843711197753,-0.171372879894276));
#19622=CARTESIAN_POINT('Ctrl Pts',(1.78000461065578,2.98198357260362,-0.013511768783165));
#19623=CARTESIAN_POINT('Ctrl Pts',(-1.52068059202578,3.11864337292237,0.144349342327946));
#19624=CARTESIAN_POINT('Ctrl Pts',(-3.44323740053193,0.434868872546417,
0.302210453439058));
#19625=CARTESIAN_POINT('Ctrl Pts',(-2.24748662857037,-2.64500439253867,
0.460071564550167));
#19626=CARTESIAN_POINT('Ctrl Pts',(0.98413688813967,-3.32800743087112,0.61793267566128));
#19627=CARTESIAN_POINT('Ctrl Pts',(3.3242675736315,-0.997273536182889,0.775793786772391));
#19628=CARTESIAN_POINT('Ctrl Pts',(2.65350107828341,2.23705783115145,0.933654897883501));
#19629=CARTESIAN_POINT('Ctrl Pts',(-0.420704297245377,3.44500822120461,
1.09151600899461));
#19630=CARTESIAN_POINT('Ctrl Pts',(-3.11384086799285,1.53272940938773,1.24937712010572));
#19631=CARTESIAN_POINT('Ctrl Pts',(-2.98662452021757,-1.76786447124123,
1.40723823121684));
#19632=CARTESIAN_POINT('Ctrl Pts',(-0.154268773033873,-3.46719137695888,
1.56509934232795));
#19633=CARTESIAN_POINT('Ctrl Pts',(2.81781362814421,-2.02612228753563,1.72296045343906));
#19634=CARTESIAN_POINT('Ctrl Pts',(3.23766264061691,1.25011350527631,1.88082156455017));
#19635=CARTESIAN_POINT('Ctrl Pts',(0.724998218776244,3.39405562633926,2.03868267566128));
#19636=CARTESIAN_POINT('Ctrl Pts',(-2.44433298400306,2.46383378430329,2.19654378677239));
#19637=CARTESIAN_POINT('Ctrl Pts',(-3.39970985401105,-0.698006346200326,
2.35440489788351));
#19638=CARTESIAN_POINT('Ctrl Pts',(-1.27579956793912,-3.22762676650925,
2.51226600899461));
#19639=CARTESIAN_POINT('Ctrl Pts',(2.00366607964198,-2.83382462640088,2.67012712010573));
#19640=CARTESIAN_POINT('Ctrl Pts',(3.46831127903076,0.12671419166248,2.82798823121683));
#19641=CARTESIAN_POINT('Ctrl Pts',(1.79153366111842,2.9724815653929,2.98584934232795));
#19642=CARTESIAN_POINT('Ctrl Pts',(-1.50792549309295,3.12592391504671,3.14371045343906));
#19643=CARTESIAN_POINT('Ctrl Pts',(-3.44158119482194,0.448060782465637,
3.30157156455017));
#19644=CARTESIAN_POINT('Ctrl Pts',(-2.25802486298351,-2.63563337612261,
3.45943267566128));
#19645=CARTESIAN_POINT('Ctrl Pts',(0.970737398643871,-3.33210271331857,
3.61729378677239));
#19646=CARTESIAN_POINT('Ctrl Pts',(3.32025430017048,-1.01052014634333,3.7751548978835));
#19647=CARTESIAN_POINT('Ctrl Pts',(2.66245099976358,2.22634100195603,3.93301600899462));
#19648=CARTESIAN_POINT('Ctrl Pts',(-0.406867188726441,3.44669387613558,
4.09087712010572));
#19649=CARTESIAN_POINT('Ctrl Pts',(-3.10766543711734,1.54520390729755,4.24873823121684));
#19650=CARTESIAN_POINT('Ctrl Pts',(-2.99369583814259,-1.75585443953709,
4.40659934232795));
#19651=CARTESIAN_POINT('Ctrl Pts',(-0.16818635164463,-3.46654769699322,
4.56446045343906));
#19652=CARTESIAN_POINT('Ctrl Pts',(2.80965791624474,-2.03741551431062,4.72232156455017));
#19653=CARTESIAN_POINT('Ctrl Pts',(3.24265463709948,1.23710569022097,4.88018267566128));
#19654=CARTESIAN_POINT('Ctrl Pts',(0.738617048059715,3.39111846455234,5.0380437867724));
#19655=CARTESIAN_POINT('Ctrl Pts',(-2.43442290318405,2.47362582310745,5.1959048978835));
#19656=CARTESIAN_POINT('Ctrl Pts',(-3.40248440570545,-0.684353310232048,
5.35376600899462));
#19657=CARTESIAN_POINT('Ctrl Pts',(-1.28874579170717,-3.22247945977245,
5.51162712010572));
#19658=CARTESIAN_POINT('Ctrl Pts',(1.99227427239527,-2.84184496548404,5.66948823121683));
#19659=CARTESIAN_POINT('Ctrl Pts',(3.46879199270663,0.112790494414327,5.82734934232795));
#19660=CARTESIAN_POINT('Ctrl Pts',(1.803451502182,2.96526596843754,5.98521045343906));
#19661=CARTESIAN_POINT('Ctrl Pts',(-1.49536511544646,3.13195190828366,6.14307156455017));
#19662=CARTESIAN_POINT('Ctrl Pts',(-3.4397548386282,0.461872530499354,6.30093267566129));
#19663=CARTESIAN_POINT('Ctrl Pts',(-2.26858675213732,-2.62654787360198,
6.45879378677239));
#19664=CARTESIAN_POINT('Ctrl Pts',(0.957353695793138,-3.33597264458916,
6.61665489788351));
#19665=CARTESIAN_POINT('Ctrl Pts',(3.31617107144768,-1.02384032406894,6.77451600899461));
#19666=CARTESIAN_POINT('Ctrl Pts',(2.67136662968815,2.21563532967061,6.93237712010573));
#19667=CARTESIAN_POINT('Ctrl Pts',(-0.393028031746144,3.44829937078522,
7.09023823121684));
#19668=CARTESIAN_POINT('Ctrl Pts',(-3.10143756889894,1.55766639256237,7.24809934232795));
#19669=CARTESIAN_POINT('Ctrl Pts',(-3.00072015011765,-1.74382285940228,
7.40596045343905));
#19670=CARTESIAN_POINT('Ctrl Pts',(-0.182100573498421,-3.46584462511342,
7.56382156455018));
#19671=CARTESIAN_POINT('Ctrl Pts',(2.80145659039814,-2.04867775807003,7.72168267566128));
#19672=CARTESIAN_POINT('Ctrl Pts',(3.24759455782818,1.22407890769377,7.8795437867724));
#19673=CARTESIAN_POINT('Ctrl Pts',(0.752223882355328,3.38812615100299,8.03740489788349));
#19674=CARTESIAN_POINT('Ctrl Pts',(-2.42447354494764,2.4833782664236,8.19526600899462));
#19675=CARTESIAN_POINT('Ctrl Pts',(-3.40520415435994,-0.670689385204343,
8.35312712010572));
#19676=CARTESIAN_POINT('Ctrl Pts',(-1.30167123501543,-3.21728015258687,
8.51098823121684));
#19677=CARTESIAN_POINT('Ctrl Pts',(1.98085035420065,-2.84981954842042,8.66884934232795));
#19678=CARTESIAN_POINT('Ctrl Pts',(3.46921681308078,0.098864999537257,8.82671045343906));
#19679=CARTESIAN_POINT('Ctrl Pts',(1.81534028008778,2.95800257805621,8.98457156455017));
#19680=CARTESIAN_POINT('Ctrl Pts',(-1.4827806401293,3.13792943795007,9.14243267566127));
#19681=CARTESIAN_POINT('Ctrl Pts',(-3.4378730539225,0.475676832953572,9.3002937867724));
#19682=CARTESIAN_POINT('Ctrl Pts',(-2.27911208446667,-2.61742004476474,
9.45815489788349));
#19683=CARTESIAN_POINT('Ctrl Pts',(0.943954565772613,-3.3397888199782,9.61601600899462));
#19684=CARTESIAN_POINT('Ctrl Pts',(3.31203440522278,-1.03714400297725,9.77387712010572));
#19685=CARTESIAN_POINT('Ctrl Pts',(2.68023921253269,2.20489395389312,9.93173823121684));
#19686=CARTESIAN_POINT('Ctrl Pts',(-0.379182541400898,3.44984929882113,
10.0895993423279));
#19687=CARTESIAN_POINT('Ctrl Pts',(-3.09515972337558,1.57010377716378,10.2474604534391));
#19688=CARTESIAN_POINT('Ctrl Pts',(-3.00769610777576,-1.73176317886687,
10.4053215645502));
#19689=CARTESIAN_POINT('Ctrl Pts',(-0.196011860918037,-3.46508570377902,
10.5631826756613));
#19690=CARTESIAN_POINT('Ctrl Pts',(2.79321012116224,-2.05990698897259,10.7210437867724));
#19691=CARTESIAN_POINT('Ctrl Pts',(3.25248214612884,1.2110324001305,10.8789048978835));
#19692=CARTESIAN_POINT('Ctrl Pts',(0.765818594962506,3.38507924024569,11.0367660089946));
#19693=CARTESIAN_POINT('Ctrl Pts',(-2.41448511783304,2.49309069223908,11.1946271201057));
#19694=CARTESIAN_POINT('Ctrl Pts',(-3.40786903136843,-0.657014653010787,
11.3524882312168));
#19695=CARTESIAN_POINT('Ctrl Pts',(-1.3145757016765,-3.21202900045202,11.510349342328));
#19696=CARTESIAN_POINT('Ctrl Pts',(1.96939451380669,-2.85774821044889,11.668210453439));
#19697=CARTESIAN_POINT('Ctrl Pts',(3.46958573405997,0.0849379149034097,
11.8260715645502));
#19698=CARTESIAN_POINT('Ctrl Pts',(1.82719979676502,2.95069151525923,11.9839326756613));
#19699=CARTESIAN_POINT('Ctrl Pts',(-1.47017225488226,3.14385641459579,12.1417937867724));
#19700=CARTESIAN_POINT('Ctrl Pts',(-3.43593590116163,0.489473446687968,
12.2996548978835));
#19701=CARTESIAN_POINT('Ctrl Pts',(-2.28960063207268,-2.60824999320481,
12.4575160089946));
#19702=CARTESIAN_POINT('Ctrl Pts',(0.930540112760845,-3.34355126315401,
12.6153771201057));
#19703=CARTESIAN_POINT('Ctrl Pts',(3.30784458181684,-1.05043080491032,12.7732382312169));
#19704=CARTESIAN_POINT('Ctrl Pts',(2.68906819704165,2.19411673426304,12.9310993423279));
#19705=CARTESIAN_POINT('Ctrl Pts',(-0.365330160772045,3.45134423437463,
13.0889604534391));
#19706=CARTESIAN_POINT('Ctrl Pts',(-3.08883349189378,1.58251471600082,13.2468215645502));
#19707=CARTESIAN_POINT('Ctrl Pts',(-3.01462075186278,-1.71967340539697,
13.4046826756613));
#19708=CARTESIAN_POINT('Ctrl Pts',(-0.209925428309919,-3.46427512302224,
13.5625437867724));
#19709=CARTESIAN_POINT('Ctrl Pts',(2.78492903121011,-2.07109504482717,13.7204048978835));
#19710=CARTESIAN_POINT('Ctrl Pts',(3.25729747472216,1.19795113049603,13.8782660089946));
#19711=CARTESIAN_POINT('Ctrl Pts',(0.779438885227093,3.38200690959721,14.0361271201057));
#19712=CARTESIAN_POINT('Ctrl Pts',(-2.40453022224261,2.50270729758603,14.1939882312168));
#19713=CARTESIAN_POINT('Ctrl Pts',(-3.41034060095634,-0.643223025084935,
14.351849342328));
#19714=CARTESIAN_POINT('Ctrl Pts',(-1.3277234162215,-3.20692920286191,14.5097104534391));
#19715=CARTESIAN_POINT('Ctrl Pts',(1.95841253548915,-2.86524258546647,14.6675715645502));
#19716=CARTESIAN_POINT('Ctrl Pts',(3.46892903525912,0.0702659147297645,
14.8254326756613));
#19717=CARTESIAN_POINT('Ctrl Pts',(1.8409162673649,2.94476989555806,14.9832937867724));
#19718=CARTESIAN_POINT('Ctrl Pts',(-1.46144261101867,3.14684084841223,15.1411548978835));
#19719=CARTESIAN_POINT('Ctrl Pts',(-2.76985851330384,1.3890220685151,15.2463956386242));
#19720=CARTESIAN_POINT('Ctrl Pts',(-2.91090525077878,0.426608275808748,
15.2990160089946));
#19721=CARTESIAN_POINT('Ctrl Pts',(1.59774743137963,-2.24059110187414,-0.219489327336926));
#19722=CARTESIAN_POINT('Ctrl Pts',(2.33853958862414,-1.71233819332979,-0.166868956966556));
#19723=CARTESIAN_POINT('Ctrl Pts',(3.24298000926863,0.127066816079881,-0.061628216225815));
#19724=CARTESIAN_POINT('Ctrl Pts',(1.66499808117169,2.78931689094975,0.0962328948852963));
#19725=CARTESIAN_POINT('Ctrl Pts',(-1.42242905026252,2.9171470684346,0.254094005996407));
#19726=CARTESIAN_POINT('Ctrl Pts',(-3.22076899721748,0.406771889250497,
0.411955117107519));
#19727=CARTESIAN_POINT('Ctrl Pts',(-2.10227597256058,-2.4741100174146,0.56981622821863));
#19728=CARTESIAN_POINT('Ctrl Pts',(0.9205515651778,-3.11298406383574,0.72767733932974));
#19729=CARTESIAN_POINT('Ctrl Pts',(3.10948583967916,-0.932839451205724,
0.885538450440853));
#19730=CARTESIAN_POINT('Ctrl Pts',(2.48205773023319,2.09252098227156,1.04339956155196));
#19731=CARTESIAN_POINT('Ctrl Pts',(-0.393522490594119,3.22242540473713,
1.20126067266308));
#19732=CARTESIAN_POINT('Ctrl Pts',(-2.91265485451303,1.43369939061326,1.35912178377418));
#19733=CARTESIAN_POINT('Ctrl Pts',(-2.79365798581306,-1.65364231910831,
1.5169828948853));
#19734=CARTESIAN_POINT('Ctrl Pts',(-0.144301430203291,-3.24317530141947,
1.67484400599641));
#19735=CARTESIAN_POINT('Ctrl Pts',(2.6357540064074,-1.8952140352733,1.83270511710752));
#19736=CARTESIAN_POINT('Ctrl Pts',(3.02847647238534,1.16934336859111,1.99056622821863));
#19737=CARTESIAN_POINT('Ctrl Pts',(0.67815590807408,3.17476486938028,2.14842733932974));
#19738=CARTESIAN_POINT('Ctrl Pts',(-2.28640403724036,2.30464488610489,2.30628845044085));
#19739=CARTESIAN_POINT('Ctrl Pts',(-3.18005377603123,-0.652907986929923,
2.46414956155196));
#19740=CARTESIAN_POINT('Ctrl Pts',(-1.19336984851725,-3.01908901853714,
2.62201067266307));
#19741=CARTESIAN_POINT('Ctrl Pts',(1.87420872841654,-2.65073053018457,2.77987178377419));
#19742=CARTESIAN_POINT('Ctrl Pts',(3.24422284634695,0.118527157015377,2.9377328948853));
#19743=CARTESIAN_POINT('Ctrl Pts',(1.67578223688854,2.78042881072881,3.09559400599641));
#19744=CARTESIAN_POINT('Ctrl Pts',(-1.41049806136441,2.92395721296701,3.25345511710752));
#19745=CARTESIAN_POINT('Ctrl Pts',(-3.21921979935999,0.419111466671254,
3.41131622821863));
#19746=CARTESIAN_POINT('Ctrl Pts',(-2.11213332909314,-2.46534446464132,
3.56917733932974));
#19747=CARTESIAN_POINT('Ctrl Pts',(0.908017819947236,-3.11681474909129,
3.72703845044085));
#19748=CARTESIAN_POINT('Ctrl Pts',(3.10573186478955,-0.94523019467185,3.88489956155197));
#19749=CARTESIAN_POINT('Ctrl Pts',(2.49042939511648,2.08249657000891,4.04276067266307));
#19750=CARTESIAN_POINT('Ctrl Pts',(-0.380579401011611,3.2240021490943,4.20062178377419));
#19751=CARTESIAN_POINT('Ctrl Pts',(-2.90687841972373,1.44536790818848,4.3584828948853));
#19752=CARTESIAN_POINT('Ctrl Pts',(-2.8002724241724,-1.64240825846459,4.5163440059964));
#19753=CARTESIAN_POINT('Ctrl Pts',(-0.157319790685473,-3.24257320977247,
4.67420511710753));
#19754=CARTESIAN_POINT('Ctrl Pts',(2.62812523703122,-1.90577760392813,4.83206622821863));
#19755=CARTESIAN_POINT('Ctrl Pts',(3.03314593476479,1.15717599162043,4.98992733932975));
#19756=CARTESIAN_POINT('Ctrl Pts',(0.690894821495446,3.17201747832858,5.14778845044085));
#19757=CARTESIAN_POINT('Ctrl Pts',(-2.27713424914591,2.31380425890769,5.30564956155197));
#19758=CARTESIAN_POINT('Ctrl Pts',(-3.18264906326793,-0.640137076925948,
5.46351067266308));
#19759=CARTESIAN_POINT('Ctrl Pts',(-1.20547961362863,-3.01427428053665,
5.62137178377419));
#19760=CARTESIAN_POINT('Ctrl Pts',(1.86355294859817,-2.65823267321491,5.7792328948853));
#19761=CARTESIAN_POINT('Ctrl Pts',(3.24467250099567,0.105503073222438,5.93709400599641));
#19762=CARTESIAN_POINT('Ctrl Pts',(1.68693006335134,2.77367941524228,6.09495511710752));
#19763=CARTESIAN_POINT('Ctrl Pts',(-1.39874921276312,2.92959573609933,6.25281622821863));
#19764=CARTESIAN_POINT('Ctrl Pts',(-3.21751144448276,0.432030834315646,
6.41067733932974));
#19765=CARTESIAN_POINT('Ctrl Pts',(-2.12201281202782,-2.45684597864148,
6.56853845044085));
#19766=CARTESIAN_POINT('Ctrl Pts',(0.895498841382776,-3.12043464316416,
6.72639956155197));
#19767=CARTESIAN_POINT('Ctrl Pts',(3.10191245446456,-0.957689752484927,
6.88426067266308));
#19768=CARTESIAN_POINT('Ctrl Pts',(2.4987689840299,2.07248259380561,7.04212178377418));
#19769=CARTESIAN_POINT('Ctrl Pts',(-0.367634395319329,3.22550391234535,
7.1999828948853));
#19770=CARTESIAN_POINT('Ctrl Pts',(-2.90105293558095,1.45702518925863,7.3578440059964));
#19771=CARTESIAN_POINT('Ctrl Pts',(-2.8068428936476,-1.63115404163953,7.51570511710752));
#19772=CARTESIAN_POINT('Ctrl Pts',(-0.170335011291572,-3.24191556353729,
7.67356622821863));
#19773=CARTESIAN_POINT('Ctrl Pts',(2.62045380083611,-1.91631219138755,7.83142733932975));
#19774=CARTESIAN_POINT('Ctrl Pts',(3.03776668601744,1.14499087267086,7.98928845044085));
#19775=CARTESIAN_POINT('Ctrl Pts',(0.703622514928034,3.16921849888318,8.14714956155197));
#19776=CARTESIAN_POINT('Ctrl Pts',(-2.26782772135753,2.32292659449655,8.30501067266308));
#19777=CARTESIAN_POINT('Ctrl Pts',(-3.18519308830241,-0.627355981407313,
8.46287178377418));
#19778=CARTESIAN_POINT('Ctrl Pts',(-1.21756994091078,-3.00941090184898,
8.62073289488531));
#19779=CARTESIAN_POINT('Ctrl Pts',(1.852867132528,-2.6656920164142,8.77859400599641));
#19780=CARTESIAN_POINT('Ctrl Pts',(3.24506987362244,0.0924773079458306,
8.93645511710752));
#19781=CARTESIAN_POINT('Ctrl Pts',(1.698050704434,2.7668853142746,9.09431622821864));
#19782=CARTESIAN_POINT('Ctrl Pts',(-1.3869778234475,2.93518705612466,9.25217733932973));
#19783=CARTESIAN_POINT('Ctrl Pts',(-3.21575124234316,0.444943237441223,
9.41003845044086));
#19784=CARTESIAN_POINT('Ctrl Pts',(-2.13185810008334,-2.44830790103859,
9.56789956155196));
#19785=CARTESIAN_POINT('Ctrl Pts',(0.882965432401702,-3.12400425453603,
9.72576067266308));
#19786=CARTESIAN_POINT('Ctrl Pts',(3.09804305924746,-0.970133877473286,
9.88362178377418));
#19787=CARTESIAN_POINT('Ctrl Pts',(2.50706830714555,2.06243522092151,10.0414828948853));
#19788=CARTESIAN_POINT('Ctrl Pts',(-0.354683465462343,3.22695369915506,
10.1993440059964));
#19789=CARTESIAN_POINT('Ctrl Pts',(-2.89518070317902,1.4686589914253,10.3572051171075));
#19790=CARTESIAN_POINT('Ctrl Pts',(-2.81336813298999,-1.61987353998757,
10.5150662282186));
#19791=CARTESIAN_POINT('Ctrl Pts',(-0.183347487058001,-3.24120567629433,
10.6729273393297));
#19792=CARTESIAN_POINT('Ctrl Pts',(2.61274013797703,-1.9268158989588,10.8307884504409));
#19793=CARTESIAN_POINT('Ctrl Pts',(3.04233848605292,1.13278730312457,10.988649561552));
#19794=CARTESIAN_POINT('Ctrl Pts',(0.716338869857416,3.16636844976869,11.1465106726631));
#19795=CARTESIAN_POINT('Ctrl Pts',(-2.25848464894066,2.33201149812516,11.3043717837742));
#19796=CARTESIAN_POINT('Ctrl Pts',(-3.18768578696123,-0.61456477697643,
11.4622328948853));
#19797=CARTESIAN_POINT('Ctrl Pts',(-1.22964064685199,-3.00449902792679,
11.6200940059964));
#19798=CARTESIAN_POINT('Ctrl Pts',(1.84215145675955,-2.67310840566659,11.7779551171075));
#19799=CARTESIAN_POINT('Ctrl Pts',(3.24541495852771,0.0794500556270124,
11.9358162282186));
#19800=CARTESIAN_POINT('Ctrl Pts',(1.70914397486321,2.76004662101762,12.0936773393297));
#19801=CARTESIAN_POINT('Ctrl Pts',(-1.37518406902836,2.94073108937221,12.2515384504409));
#19802=CARTESIAN_POINT('Ctrl Pts',(-3.21393924949186,0.457848448617044,
12.409399561552));
#19803=CARTESIAN_POINT('Ctrl Pts',(-2.14166898008542,-2.43973032873338,
12.5672606726631));
#19804=CARTESIAN_POINT('Ctrl Pts',(0.870417690451563,-3.12752360534598,
12.7251217837742));
#19805=CARTESIAN_POINT('Ctrl Pts',(3.09412394134766,-0.98256221591188,12.8829828948853));
#19806=CARTESIAN_POINT('Ctrl Pts',(2.51532684882466,2.05235432006483,13.0408440059964));
#19807=CARTESIAN_POINT('Ctrl Pts',(-0.341726090504644,3.22835204655998,
13.1987051171075));
#19808=CARTESIAN_POINT('Ctrl Pts',(-2.88926321104715,1.48026805649486,13.3565662282186));
#19809=CARTESIAN_POINT('Ctrl Pts',(-2.81984537414356,-1.60856488971291,
13.5144273393297));
#19810=CARTESIAN_POINT('Ctrl Pts',(-0.196362095487134,-3.24044746735677,
13.6722884504409));
#19811=CARTESIAN_POINT('Ctrl Pts',(2.60499409125458,-1.93728109181189,13.830149561552));
#19812=CARTESIAN_POINT('Ctrl Pts',(3.04684269509828,1.12055121749295,13.9880106726631));
#19813=CARTESIAN_POINT('Ctrl Pts',(0.729079149865556,3.16349462314833,14.1458717837742));
#19814=CARTESIAN_POINT('Ctrl Pts',(-2.24917294156805,2.34100677226896,14.3037328948853));
#19815=CARTESIAN_POINT('Ctrl Pts',(-3.1899976678388,-0.601664229474863,
14.4615940059964));
#19816=CARTESIAN_POINT('Ctrl Pts',(-1.24193888437236,-2.9997287294955,14.6194551171075));
#19817=CARTESIAN_POINT('Ctrl Pts',(1.83187902672385,-2.68011856729716,14.7773162282186));
#19818=CARTESIAN_POINT('Ctrl Pts',(3.24480068919561,0.0657260169420378,
14.9351773393297));
#19819=CARTESIAN_POINT('Ctrl Pts',(1.72197422097186,2.75450759860113,15.0930384504409));
#19820=CARTESIAN_POINT('Ctrl Pts',(-1.36701844957144,2.94352269819615,15.250899561552));
#19821=CARTESIAN_POINT('Ctrl Pts',(-2.59089728316432,1.29927701587847,15.3561403022927));
#19822=CARTESIAN_POINT('Ctrl Pts',(-2.72283095673204,0.399045011670964,
15.4087606726631));
#19823=CARTESIAN_POINT('Ctrl Pts',(1.48738611075532,-2.0858265952159,-0.109744663668465));
#19824=CARTESIAN_POINT('Ctrl Pts',(2.17700947925639,-1.59406173695134,-0.0571242932980945));
#19825=CARTESIAN_POINT('Ctrl Pts',(3.01897742315769,0.118289920962009,0.0481164474426461));
#19826=CARTESIAN_POINT('Ctrl Pts',(1.5499915516876,2.59665020929587,0.205977558553758));
#19827=CARTESIAN_POINT('Ctrl Pts',(-1.32417750849926,2.71565076394683,0.363838669664868));
#19828=CARTESIAN_POINT('Ctrl Pts',(-2.99830059390304,0.37867490595458,0.521699780775981));
#19829=CARTESIAN_POINT('Ctrl Pts',(-1.95706531655079,-2.30321564229053,
0.679560891887089));
#19830=CARTESIAN_POINT('Ctrl Pts',(0.856966242215927,-2.89796069680035,
0.837422002998203));
#19831=CARTESIAN_POINT('Ctrl Pts',(2.89470410572683,-0.86840536622856,0.995283114109312));
#19832=CARTESIAN_POINT('Ctrl Pts',(2.31061438218297,1.94798413339166,1.15314422522042));
#19833=CARTESIAN_POINT('Ctrl Pts',(-0.36634068394286,2.99984258826965,1.31100533633153));
#19834=CARTESIAN_POINT('Ctrl Pts',(-2.71146884103322,1.33466937183879,1.46886644744265));
#19835=CARTESIAN_POINT('Ctrl Pts',(-2.60069145140856,-1.53942016697539,
1.62672755855376));
#19836=CARTESIAN_POINT('Ctrl Pts',(-0.134334087372704,-3.01915922588007,
1.78458866966487));
#19837=CARTESIAN_POINT('Ctrl Pts',(2.45369438467058,-1.76430578301097,1.94244978077598));
#19838=CARTESIAN_POINT('Ctrl Pts',(2.81929030415377,1.0885732319059,2.10031089188709));
#19839=CARTESIAN_POINT('Ctrl Pts',(0.63131359737191,2.95547411242131,2.2581720029982));
#19840=CARTESIAN_POINT('Ctrl Pts',(-2.12847509047765,2.14545598790649,2.41603311410931));
#19841=CARTESIAN_POINT('Ctrl Pts',(-2.96039769805142,-0.607809627659522,
2.57389422522043));
#19842=CARTESIAN_POINT('Ctrl Pts',(-1.11094012909538,-2.81055127056503,
2.73175533633153));
#19843=CARTESIAN_POINT('Ctrl Pts',(1.74475137719111,-2.46763643396825,2.88961644744264));
#19844=CARTESIAN_POINT('Ctrl Pts',(3.02013441366314,0.110340122368272,3.04747755855376));
#19845=CARTESIAN_POINT('Ctrl Pts',(1.56003081265866,2.58837605606472,3.20533866966487));
#19846=CARTESIAN_POINT('Ctrl Pts',(-1.31307062963587,2.72199051088731,3.36319978077598));
#19847=CARTESIAN_POINT('Ctrl Pts',(-2.99685840389804,0.390162150876873,
3.52106089188709));
#19848=CARTESIAN_POINT('Ctrl Pts',(-1.96624179520275,-2.29505555316004,
3.6789220029982));
#19849=CARTESIAN_POINT('Ctrl Pts',(0.845298241250599,-2.90152678486402,
3.83678311410932));
#19850=CARTESIAN_POINT('Ctrl Pts',(2.89120942940861,-0.879940243000373,
3.99464422522043));
#19851=CARTESIAN_POINT('Ctrl Pts',(2.31840779046938,1.93865213806179,4.15250533633154));
#19852=CARTESIAN_POINT('Ctrl Pts',(-0.354291613296782,3.00131042205302,
4.31036644744265));
#19853=CARTESIAN_POINT('Ctrl Pts',(-2.70609140233011,1.34553190907942,4.46822755855376));
#19854=CARTESIAN_POINT('Ctrl Pts',(-2.60684901020221,-1.52896207739209,
4.62608866966487));
#19855=CARTESIAN_POINT('Ctrl Pts',(-0.146453229726317,-3.01859872255171,
4.78394978077598));
#19856=CARTESIAN_POINT('Ctrl Pts',(2.44659255781772,-1.77413969354566,4.94181089188709));
#19857=CARTESIAN_POINT('Ctrl Pts',(2.82363723243009,1.07724629301989,5.09967200299821));
#19858=CARTESIAN_POINT('Ctrl Pts',(0.643172594931182,2.95291649210482,5.25753311410931));
#19859=CARTESIAN_POINT('Ctrl Pts',(-2.11984559510778,2.15398269470792,5.41539422522043));
#19860=CARTESIAN_POINT('Ctrl Pts',(-2.96281372083041,-0.595920843619846,
5.57325533633153));
#19861=CARTESIAN_POINT('Ctrl Pts',(-1.12221343555009,-2.80606910130085,
5.73111644744265));
#19862=CARTESIAN_POINT('Ctrl Pts',(1.73483162480106,-2.47462038094578,5.88897755855376));
#19863=CARTESIAN_POINT('Ctrl Pts',(3.02055300928471,0.0982156520305535,
6.04683866966487));
#19864=CARTESIAN_POINT('Ctrl Pts',(1.57040862452068,2.58209286204701,6.20469978077598));
#19865=CARTESIAN_POINT('Ctrl Pts',(-1.30213331007977,2.72723956391501,6.36256089188709));
#19866=CARTESIAN_POINT('Ctrl Pts',(-2.99526805033731,0.402189138131933,
6.52042200299821));
#19867=CARTESIAN_POINT('Ctrl Pts',(-1.97543887191833,-2.28714408368097,
6.67828311410931));
#19868=CARTESIAN_POINT('Ctrl Pts',(0.833643986972413,-2.90489664173917,
6.83614422522043));
#19869=CARTESIAN_POINT('Ctrl Pts',(2.88765383748144,-0.891539180900916,
6.99400533633154));
#19870=CARTESIAN_POINT('Ctrl Pts',(2.32617133837164,1.9293298579406,7.15186644744265));
#19871=CARTESIAN_POINT('Ctrl Pts',(-0.342240758892514,3.00270845390548,
7.30972755855377));
#19872=CARTESIAN_POINT('Ctrl Pts',(-2.70066830226297,1.35638398595488,7.46758866966487));
#19873=CARTESIAN_POINT('Ctrl Pts',(-2.61296563717754,-1.51848522387679,
7.62544978077598));
#19874=CARTESIAN_POINT('Ctrl Pts',(-0.158569449084724,-3.01798650196116,
7.78331089188708));
#19875=CARTESIAN_POINT('Ctrl Pts',(2.43945101127409,-1.78394662470507,7.94117200299821));
#19876=CARTESIAN_POINT('Ctrl Pts',(2.8279388142067,1.06590283764795,8.09903311410931));
#19877=CARTESIAN_POINT('Ctrl Pts',(0.655021147500741,2.95031084676337,8.25689422522044));
#19878=CARTESIAN_POINT('Ctrl Pts',(-2.11118189776743,2.16247492256949,8.41475533633153));
#19879=CARTESIAN_POINT('Ctrl Pts',(-2.96518202224487,-0.584022577610279,
8.57261644744266));
#19880=CARTESIAN_POINT('Ctrl Pts',(-1.13346864680612,-2.8015416511111,8.73047755855375));
#19881=CARTESIAN_POINT('Ctrl Pts',(1.72488391085535,-2.48156448440799,8.88833866966489));
#19882=CARTESIAN_POINT('Ctrl Pts',(3.0209229341641,0.0860896163543999,9.04619978077597));
#19883=CARTESIAN_POINT('Ctrl Pts',(1.58076112878023,2.575768050493,9.2040608918871));
#19884=CARTESIAN_POINT('Ctrl Pts',(-1.2911750067657,2.73244467429924,9.3619220029982));
#19885=CARTESIAN_POINT('Ctrl Pts',(-2.99362943076381,0.414209641928883,
9.51978311410932));
#19886=CARTESIAN_POINT('Ctrl Pts',(-1.98460411570002,-2.27919575731244,
9.67764422522042));
#19887=CARTESIAN_POINT('Ctrl Pts',(0.821976299030791,-2.90821968909385,
9.83550533633154));
#19888=CARTESIAN_POINT('Ctrl Pts',(2.88405171327213,-0.903123751969326,
9.99336644744264));
#19889=CARTESIAN_POINT('Ctrl Pts',(2.33389740175841,1.9199764879499,10.1512275585538));
#19890=CARTESIAN_POINT('Ctrl Pts',(-0.330184389523787,3.00405809948898,
10.3090886696649));
#19891=CARTESIAN_POINT('Ctrl Pts',(-2.69520168298246,1.36721420568682,10.466949780776));
#19892=CARTESIAN_POINT('Ctrl Pts',(-2.61904015820422,-1.50798390110827,
10.6248108918871));
#19893=CARTESIAN_POINT('Ctrl Pts',(-0.170683113197963,-3.01732564880962,
10.7826720029982));
#19894=CARTESIAN_POINT('Ctrl Pts',(2.43227015479182,-1.793724808945,10.9405331141093));
#19895=CARTESIAN_POINT('Ctrl Pts',(2.83219482597701,1.05454220611865,11.0983942252204));
#19896=CARTESIAN_POINT('Ctrl Pts',(0.666859144752323,2.94765765929168,11.2562553363315));
#19897=CARTESIAN_POINT('Ctrl Pts',(-2.10248418004828,2.17093230401124,11.4141164474427));
#19898=CARTESIAN_POINT('Ctrl Pts',(-2.96750254255404,-0.572114900942073,
11.5719775585538));
#19899=CARTESIAN_POINT('Ctrl Pts',(-1.14470559202747,-2.79696905540156,
11.7298386696649));
#19900=CARTESIAN_POINT('Ctrl Pts',(1.7149083997124,-2.48846860088429,11.887699780776));
#19901=CARTESIAN_POINT('Ctrl Pts',(3.02124418299545,0.0739621963506113,
12.0455608918871));
#19902=CARTESIAN_POINT('Ctrl Pts',(1.5910881529614,2.56940172677601,12.2034220029982));
#19903=CARTESIAN_POINT('Ctrl Pts',(-1.28019588317448,2.73760576414863,12.3612831141093));
#19904=CARTESIAN_POINT('Ctrl Pts',(-2.99194259782208,0.42622345054612,12.5191442252204));
#19905=CARTESIAN_POINT('Ctrl Pts',(-1.99373732809816,-2.27121066426194,
12.6770053363315));
#19906=CARTESIAN_POINT('Ctrl Pts',(0.810295268142284,-2.91149594753796,
12.8348664474426));
#19907=CARTESIAN_POINT('Ctrl Pts',(2.88040330087848,-0.914693626913434,
12.9927275585538));
#19908=CARTESIAN_POINT('Ctrl Pts',(2.34158550060768,1.91059190586663,13.1505886696649));
#19909=CARTESIAN_POINT('Ctrl Pts',(-0.318122020237242,3.00535985874532,
13.308449780776));
#19910=CARTESIAN_POINT('Ctrl Pts',(-2.68969293020052,1.37802139698889,13.4663108918871));
#19911=CARTESIAN_POINT('Ctrl Pts',(-2.62506999642434,-1.49745637402886,
13.6241720029982));
#19912=CARTESIAN_POINT('Ctrl Pts',(-0.182798762664348,-3.0166198116913,
13.7820331141093));
#19913=CARTESIAN_POINT('Ctrl Pts',(2.42505915129906,-1.80346713879661,13.9398942252204));
#19914=CARTESIAN_POINT('Ctrl Pts',(2.8363879154744,1.04315130448987,14.0977553363316));
#19915=CARTESIAN_POINT('Ctrl Pts',(0.678719414504022,2.94498233669946,14.2556164474426));
#19916=CARTESIAN_POINT('Ctrl Pts',(-2.09381566089348,2.17930624695187,14.4134775585538));
#19917=CARTESIAN_POINT('Ctrl Pts',(-2.96965473472126,-0.560105433864789,
14.5713386696649));
#19918=CARTESIAN_POINT('Ctrl Pts',(-1.15615435252323,-2.79252825612909,
14.729199780776));
#19919=CARTESIAN_POINT('Ctrl Pts',(1.70534551795855,-2.49499454912784,14.8870608918871));
#19920=CARTESIAN_POINT('Ctrl Pts',(3.0206723431321,0.0611861191543108,15.0449220029982));
#19921=CARTESIAN_POINT('Ctrl Pts',(1.60303217457882,2.56424530164419,15.2027831141093));
#19922=CARTESIAN_POINT('Ctrl Pts',(-1.27259428812422,2.74020454798006,15.3606442252204));
#19923=CARTESIAN_POINT('Ctrl Pts',(-2.41193605302479,1.20953196324185,15.4658849659612));
#19924=CARTESIAN_POINT('Ctrl Pts',(-2.53475666268529,0.371481747533179,
15.5185053363315));
#19925=CARTESIAN_POINT('Ctrl Pts',(1.37702479013102,-1.93106208855765,-3.60822483003176E-15));
#19926=CARTESIAN_POINT('Ctrl Pts',(2.01547936988864,-1.47578528057288,0.0526203703703667));
#19927=CARTESIAN_POINT('Ctrl Pts',(2.79497483704674,0.109513025844136,0.157861111111108));
#19928=CARTESIAN_POINT('Ctrl Pts',(1.4349850222035,2.40398352764199,0.315722222222219));
#19929=CARTESIAN_POINT('Ctrl Pts',(-1.225925966736,2.51415445945906,0.473583333333329));
#19930=CARTESIAN_POINT('Ctrl Pts',(-2.77583219058859,0.350577922658662,
0.631444444444441));
#19931=CARTESIAN_POINT('Ctrl Pts',(-1.811854660541,-2.13232126716645,0.789305555555552));
#19932=CARTESIAN_POINT('Ctrl Pts',(0.793380919254056,-2.68293732976497,
0.947166666666663));
#19933=CARTESIAN_POINT('Ctrl Pts',(2.67992237177449,-0.803971281251394,
1.10502777777777));
#19934=CARTESIAN_POINT('Ctrl Pts',(2.13917103413275,1.80344728451176,1.26288888888888));
#19935=CARTESIAN_POINT('Ctrl Pts',(-0.339158877291603,2.77725977180218,
1.42075));
#19936=CARTESIAN_POINT('Ctrl Pts',(-2.51028282755341,1.23563935306431,1.57861111111111));
#19937=CARTESIAN_POINT('Ctrl Pts',(-2.40772491700405,-1.42519801484247,
1.73647222222222));
#19938=CARTESIAN_POINT('Ctrl Pts',(-0.124366744542119,-2.79514315034066,
1.89433333333333));
#19939=CARTESIAN_POINT('Ctrl Pts',(2.27163476293377,-1.63339753074864,2.05219444444444));
#19940=CARTESIAN_POINT('Ctrl Pts',(2.61010413592219,1.00780309522069,2.21005555555555));
#19941=CARTESIAN_POINT('Ctrl Pts',(0.584471286669745,2.73618335546233,2.36791666666667));
#19942=CARTESIAN_POINT('Ctrl Pts',(-1.97054614371495,1.98626708970809,2.52577777777777));
#19943=CARTESIAN_POINT('Ctrl Pts',(-2.7407416200716,-0.562711268389121,
2.68363888888889));
#19944=CARTESIAN_POINT('Ctrl Pts',(-1.02851040967351,-2.60201352259292,
2.84149999999999));
#19945=CARTESIAN_POINT('Ctrl Pts',(1.61529402596567,-2.28454233775194,2.99936111111111));
#19946=CARTESIAN_POINT('Ctrl Pts',(2.79604598097933,0.102153087721166,3.15722222222222));
#19947=CARTESIAN_POINT('Ctrl Pts',(1.44427938842878,2.39632330140064,3.31508333333333));
#19948=CARTESIAN_POINT('Ctrl Pts',(-1.21564319790733,2.5200238088076,3.47294444444445));
#19949=CARTESIAN_POINT('Ctrl Pts',(-2.77449700843608,0.361212835082494,
3.63080555555555));
#19950=CARTESIAN_POINT('Ctrl Pts',(-1.82035026131238,-2.12476664167876,
3.78866666666667));
#19951=CARTESIAN_POINT('Ctrl Pts',(0.782578662553965,-2.68623882063674,
3.94652777777777));
#19952=CARTESIAN_POINT('Ctrl Pts',(2.67668699402767,-0.814650291328897,
4.10438888888889));
#19953=CARTESIAN_POINT('Ctrl Pts',(2.14638618582228,1.79480770611467,4.26225));
#19954=CARTESIAN_POINT('Ctrl Pts',(-0.328003825581952,2.77861869501174,
4.42011111111111));
#19955=CARTESIAN_POINT('Ctrl Pts',(-2.50530438493649,1.24569590997036,4.57797222222222));
#19956=CARTESIAN_POINT('Ctrl Pts',(-2.41342559623202,-1.41551589631959,
4.73583333333333));
#19957=CARTESIAN_POINT('Ctrl Pts',(-0.135586668767159,-2.79462423533096,
4.89369444444444));
#19958=CARTESIAN_POINT('Ctrl Pts',(2.2650598786042,-1.64250178316317,5.05155555555556));
#19959=CARTESIAN_POINT('Ctrl Pts',(2.61412853009539,0.997316594419356,5.20941666666666));
#19960=CARTESIAN_POINT('Ctrl Pts',(0.595450368366912,2.73381550588105,5.36727777777778));
#19961=CARTESIAN_POINT('Ctrl Pts',(-1.96255694106964,1.99416113050815,5.52513888888888));
#19962=CARTESIAN_POINT('Ctrl Pts',(-2.74297837839289,-0.551704610313744,
5.683));
#19963=CARTESIAN_POINT('Ctrl Pts',(-1.03894725747156,-2.59786392206505,
5.84086111111111));
#19964=CARTESIAN_POINT('Ctrl Pts',(1.60611030100396,-2.29100808867664,5.99872222222222));
#19965=CARTESIAN_POINT('Ctrl Pts',(2.79643351757374,0.090928230838667,6.15658333333333));
#19966=CARTESIAN_POINT('Ctrl Pts',(1.45388718569001,2.39050630885174,6.31444444444444));
#19967=CARTESIAN_POINT('Ctrl Pts',(-1.20551740739643,2.52488339173069,6.47230555555556));
#19968=CARTESIAN_POINT('Ctrl Pts',(-2.77302465619186,0.372347441948222,
6.63016666666666));
#19969=CARTESIAN_POINT('Ctrl Pts',(-1.82886493180883,-2.11744218872047,
6.78802777777778));
#19970=CARTESIAN_POINT('Ctrl Pts',(0.771789132562049,-2.68935864031417,
6.94588888888888));
#19971=CARTESIAN_POINT('Ctrl Pts',(2.67339522049833,-0.825388609316905,
7.10375));
#19972=CARTESIAN_POINT('Ctrl Pts',(2.15357369271338,1.7861771220756,7.26161111111111));
#19973=CARTESIAN_POINT('Ctrl Pts',(-0.3168471224657,2.77991299546561,7.41947222222222));
#19974=CARTESIAN_POINT('Ctrl Pts',(-2.50028366894498,1.25574278265114,7.57733333333334));
#19975=CARTESIAN_POINT('Ctrl Pts',(-2.41908838070749,-1.40581640611404,
7.73519444444443));
#19976=CARTESIAN_POINT('Ctrl Pts',(-0.146803886877873,-2.79405744038503,
7.89305555555557));
#19977=CARTESIAN_POINT('Ctrl Pts',(2.25844822171206,-1.65158105802259,8.05091666666665));
#19978=CARTESIAN_POINT('Ctrl Pts',(2.61811094239596,0.986814802625037,8.20877777777778));
#19979=CARTESIAN_POINT('Ctrl Pts',(0.606419780073446,2.73140319464357,8.36663888888888));
#19980=CARTESIAN_POINT('Ctrl Pts',(-1.95453607417732,2.00202325064244,8.52450000000001));
#19981=CARTESIAN_POINT('Ctrl Pts',(-2.74517095618734,-0.540689173813247,
8.68236111111111));
#19982=CARTESIAN_POINT('Ctrl Pts',(-1.04936735270146,-2.59367240037321,
8.84022222222223));
#19983=CARTESIAN_POINT('Ctrl Pts',(1.59690068918271,-2.29743695240177,8.99808333333332));
#19984=CARTESIAN_POINT('Ctrl Pts',(2.79677599470576,0.0797019247629725,
9.15594444444445));
#19985=CARTESIAN_POINT('Ctrl Pts',(1.46347155312646,2.38465078671139,9.31380555555555));
#19986=CARTESIAN_POINT('Ctrl Pts',(-1.19537219008389,2.52970229247383,9.47166666666666));
#19987=CARTESIAN_POINT('Ctrl Pts',(-2.77150761918447,0.383476046416537,
9.62952777777778));
#19988=CARTESIAN_POINT('Ctrl Pts',(-1.83735013131669,-2.1100836135863,9.78738888888888));
#19989=CARTESIAN_POINT('Ctrl Pts',(0.760987165659879,-2.69243512365168,
9.94525));
#19990=CARTESIAN_POINT('Ctrl Pts',(2.6700603672968,-0.836113626465368,10.1031111111111));
#19991=CARTESIAN_POINT('Ctrl Pts',(2.16072649637127,1.7775177549783,10.2609722222222));
#19992=CARTESIAN_POINT('Ctrl Pts',(-0.305685313585232,2.78116249982291,
10.4188333333333));
#19993=CARTESIAN_POINT('Ctrl Pts',(-2.4952226627859,1.26576941994835,10.5766944444444));
#19994=CARTESIAN_POINT('Ctrl Pts',(-2.42471218341845,-1.39609426222898,
10.7345555555556));
#19995=CARTESIAN_POINT('Ctrl Pts',(-0.158018739337926,-2.79344562132492,
10.8924166666667));
#19996=CARTESIAN_POINT('Ctrl Pts',(2.25180017160661,-1.66063371893121,11.0502777777778));
#19997=CARTESIAN_POINT('Ctrl Pts',(2.62205116590109,0.976297109112734,11.2081388888889));
#19998=CARTESIAN_POINT('Ctrl Pts',(0.617379419647229,2.72894686881467,11.366));
#19999=CARTESIAN_POINT('Ctrl Pts',(-1.9464837111559,2.00985310989732,11.5238611111111));
#20000=CARTESIAN_POINT('Ctrl Pts',(-2.74731929814685,-0.529665024907718,
11.6817222222222));
#20001=CARTESIAN_POINT('Ctrl Pts',(-1.05977053720295,-2.58943908287633,
11.8395833333333));
#20002=CARTESIAN_POINT('Ctrl Pts',(1.58766534266525,-2.30382879610199,11.9974444444444));
#20003=CARTESIAN_POINT('Ctrl Pts',(2.79707340746319,0.0684743370742143,
12.1553055555555));
#20004=CARTESIAN_POINT('Ctrl Pts',(1.47303233105958,2.37875683253439,12.3131666666667));
#20005=CARTESIAN_POINT('Ctrl Pts',(-1.18520769732058,2.53448043892505,12.4710277777778));
#20006=CARTESIAN_POINT('Ctrl Pts',(-2.76994594615232,0.394598452475193,
12.6288888888889));
#20007=CARTESIAN_POINT('Ctrl Pts',(-1.8458056761109,-2.1026909997905,12.78675));
#20008=CARTESIAN_POINT('Ctrl Pts',(0.750172845833004,-2.69546828972993,
12.9446111111111));
#20009=CARTESIAN_POINT('Ctrl Pts',(2.66668266040929,-0.846825037914988,
13.1024722222222));
#20010=CARTESIAN_POINT('Ctrl Pts',(2.16784415239069,1.76882949166842,13.2603333333333));
#20011=CARTESIAN_POINT('Ctrl Pts',(-0.294517949969841,2.78236767093066,
13.4181944444444));
#20012=CARTESIAN_POINT('Ctrl Pts',(-2.49012264935389,1.27577473748293,13.5760555555556));
#20013=CARTESIAN_POINT('Ctrl Pts',(-2.43029461870512,-1.3863478583448,13.7339166666666));
#20014=CARTESIAN_POINT('Ctrl Pts',(-0.16923542984156,-2.79279215602584,
13.8917777777778));
#20015=CARTESIAN_POINT('Ctrl Pts',(2.24512421134353,-1.66965318578134,14.0496388888889));
#20016=CARTESIAN_POINT('Ctrl Pts',(2.62593313585052,0.965751391486786,14.2075));
#20017=CARTESIAN_POINT('Ctrl Pts',(0.628359679142483,2.72647005025058,14.3653611111111));
#20018=CARTESIAN_POINT('Ctrl Pts',(-1.93845838021891,2.01760572163479,14.5232222222222));
#20019=CARTESIAN_POINT('Ctrl Pts',(-2.74931180160372,-0.518546638254714,
14.6810833333333));
#20020=CARTESIAN_POINT('Ctrl Pts',(-1.07036982067409,-2.58532778276268,
14.8389444444444));
#20021=CARTESIAN_POINT('Ctrl Pts',(1.57881200919325,-2.30987053095853,14.9968055555556));
#20022=CARTESIAN_POINT('Ctrl Pts',(2.79654399706859,0.0566462213665858,
15.1546666666667));
#20023=CARTESIAN_POINT('Ctrl Pts',(1.48409012818578,2.37398300468726,15.3125277777778));
#20024=CARTESIAN_POINT('Ctrl Pts',(-1.17817012667699,2.53688639776398,15.4703888888889));
#20025=CARTESIAN_POINT('Ctrl Pts',(-2.23297482288527,1.11978691060522,15.5756296296296));
#20026=CARTESIAN_POINT('Ctrl Pts',(-2.34668236863854,0.343918483395395,
15.62825));
#20027=CARTESIAN_POINT('',(1.37702479013102,-1.93106208855765,0.));
#20028=CARTESIAN_POINT('Ctrl Pts',(1.37702479013102,-1.93106208855765,-3.60822483003176E-15));
#20029=CARTESIAN_POINT('Ctrl Pts',(2.01547936988864,-1.47578528057288,0.0526203703703667));
#20030=CARTESIAN_POINT('Ctrl Pts',(2.79497483704674,0.109513025844136,0.157861111111108));
#20031=CARTESIAN_POINT('Ctrl Pts',(1.4349850222035,2.40398352764199,0.315722222222219));
#20032=CARTESIAN_POINT('Ctrl Pts',(-1.225925966736,2.51415445945906,0.473583333333329));
#20033=CARTESIAN_POINT('Ctrl Pts',(-2.32453883371355,0.980556500150706,
0.585479295290919));
#20034=CARTESIAN_POINT('Ctrl Pts',(-2.37485146083742,0.100616720091163,
0.644754886878137));
#20035=CARTESIAN_POINT('Ctrl Pts',(-2.37409249406917,0.00172857025301858,
0.651410108094986));
#20036=CARTESIAN_POINT('Ctrl Pts',(1.29200104020317,2.64812001020929,8.84708972748172E-17));
#20037=CARTESIAN_POINT('Ctrl Pts',(1.36315737313149,2.60529414881161,1.11522009070411E-16));
#20038=CARTESIAN_POINT('Ctrl Pts',(1.43224767624703,2.55934891308958,-5.0435019692162E-16));
#20039=CARTESIAN_POINT('Ctrl Pts',(1.49903325513988,2.51027466650741,-4.38885039422132E-16));
#20040=CARTESIAN_POINT('Ctrl Pts',(1.57786836962904,2.45234638450537,-3.65724347932505E-16));
#20041=CARTESIAN_POINT('Ctrl Pts',(1.65349331585608,2.39005818913334,-5.19266877679362E-16));
#20042=CARTESIAN_POINT('Ctrl Pts',(1.72573019513852,2.32378926839401,-6.48786580015326E-16));
#20043=CARTESIAN_POINT('Ctrl Pts',(1.76374109312884,2.28891869797108,-7.16939582223243E-16));
#20044=CARTESIAN_POINT('Ctrl Pts',(1.80081318017132,2.2529453987339,-5.63901193634668E-16));
#20045=CARTESIAN_POINT('Ctrl Pts',(1.83691551656788,2.21592189026143,-5.759281940243E-16));
#20046=CARTESIAN_POINT('Ctrl Pts',(1.85077163488616,2.20171222503873,-5.80544170635404E-16));
#20047=CARTESIAN_POINT('Ctrl Pts',(1.86448486767998,2.18734784556943,1.18680337545582E-16));
#20048=CARTESIAN_POINT('Ctrl Pts',(1.87805332095389,2.17283167229843,1.45716771982052E-16));
#20049=CARTESIAN_POINT('Ctrl Pts',(1.88973877018296,2.16033002584437,1.69001141656681E-16));
#20050=CARTESIAN_POINT('Ctrl Pts',(1.90131548250979,2.14771713833219,-1.20552840767492E-16));
#20051=CARTESIAN_POINT('Ctrl Pts',(1.91277473204616,2.1350036118777,-1.04083408558608E-16));
#20052=CARTESIAN_POINT('Ctrl Pts',(1.9778462733255,2.06280963801715,-1.05614606835039E-17));
#20053=CARTESIAN_POINT('Ctrl Pts',(2.03920496551099,1.98729716595704,-4.81412066085989E-16));
#20054=CARTESIAN_POINT('Ctrl Pts',(2.09668120715734,1.90884345828848,-3.33066907387547E-16));
#20055=CARTESIAN_POINT('Ctrl Pts',(2.14417843271961,1.84401087107344,-2.10477411937863E-16));
#20056=CARTESIAN_POINT('Ctrl Pts',(2.18902362087598,1.7771688452355,-1.7119245770294E-16));
#20057=CARTESIAN_POINT('Ctrl Pts',(2.23109606376114,1.7085204430367,-1.94289029309402E-16));
#20058=CARTESIAN_POINT('Ctrl Pts',(2.24950275752339,1.67848676707472,-2.0439377938723E-16));
#20059=CARTESIAN_POINT('Ctrl Pts',(2.26737842523222,1.6481072631063,-4.61788465798711E-16));
#20060=CARTESIAN_POINT('Ctrl Pts',(2.28471149018554,1.61739870311764,-5.13478148889135E-16));
#20061=CARTESIAN_POINT('Ctrl Pts',(2.29518347047447,1.59884575614786,-5.44707094486553E-16));
#20062=CARTESIAN_POINT('Ctrl Pts',(2.30545737670969,1.58017269818218,-5.13081578012294E-16));
#20063=CARTESIAN_POINT('Ctrl Pts',(2.3155304906665,1.56138322284078,-5.55111512312578E-16));
#20064=CARTESIAN_POINT('Ctrl Pts',(2.32274660107223,1.54792294341672,-5.85220637212436E-16));
#20065=CARTESIAN_POINT('Ctrl Pts',(2.32985933504635,1.5344033850802,-2.08590721469464E-17));
#20066=CARTESIAN_POINT('Ctrl Pts',(2.33686168047272,1.52083799385098,-2.77555756156289E-17));
#20067=CARTESIAN_POINT('Ctrl Pts',(2.38047027627073,1.43635663411551,-7.07050181056999E-17));
#20068=CARTESIAN_POINT('Ctrl Pts',(2.41986655819018,1.34997905359849,1.3198210981114E-16));
#20069=CARTESIAN_POINT('Ctrl Pts',(2.45488985599288,1.26205357875123,5.55111512312578E-17));
#20070=CARTESIAN_POINT('Ctrl Pts',(2.48959846523414,1.17491812491653,-2.02727065483809E-17));
#20071=CARTESIAN_POINT('Ctrl Pts',(2.52001253380174,1.08626153918075,-4.44579204063227E-16));
#20072=CARTESIAN_POINT('Ctrl Pts',(2.54592562425351,0.996413712953991,-4.9960036108132E-16));
#20073=CARTESIAN_POINT('Ctrl Pts',(2.57101139534936,0.909434430942866,-5.528648743571E-16));
#20074=CARTESIAN_POINT('Ctrl Pts',(2.59187898968551,0.821337996875181,-7.89241560757653E-18));
#20075=CARTESIAN_POINT('Ctrl Pts',(2.60829286172102,0.732427405689614,-8.32667268468867E-17));
#20076=CARTESIAN_POINT('Ctrl Pts',(2.61783087340729,0.680761945161682,-1.27066328786625E-16));
#20077=CARTESIAN_POINT('Ctrl Pts',(2.62586408863254,0.628821695636964,-4.14952786105416E-17));
#20078=CARTESIAN_POINT('Ctrl Pts',(2.63233843305125,0.576668196894126,-5.55111512312578E-17));
#20079=CARTESIAN_POINT('Ctrl Pts',(2.63414224296016,0.562137768524485,-5.94160979378542E-17));
#20080=CARTESIAN_POINT('Ctrl Pts',(2.63582527555606,0.547588319420663,3.76279563716787E-16));
#20081=CARTESIAN_POINT('Ctrl Pts',(2.63738542604938,0.533029261526728,3.60822483003176E-16));
#20082=CARTESIAN_POINT('Ctrl Pts',(2.64690685377435,0.444176924476997,2.66489610960485E-16));
#20083=CARTESIAN_POINT('Ctrl Pts',(2.65183263786108,0.355196731300303,5.62349138697447E-16));
#20084=CARTESIAN_POINT('Ctrl Pts',(2.65198717743404,0.266381980286723,3.88578058618805E-16));
#20085=CARTESIAN_POINT('Ctrl Pts',(2.65207998114243,0.213047173573617,2.84225494854879E-16));
#20086=CARTESIAN_POINT('Ctrl Pts',(2.65045121279133,0.159772024909719,-3.854419951949E-17));
#20087=CARTESIAN_POINT('Ctrl Pts',(2.64705383408491,0.106621318043217,-8.32667268468867E-17));
#20088=CARTESIAN_POINT('Ctrl Pts',(2.64128166054733,0.0163178428672467,
-1.29468843946197E-16));
#20089=CARTESIAN_POINT('Ctrl Pts',(2.63040647827402,-0.0736278476965388,
-4.84995897836269E-16));
#20090=CARTESIAN_POINT('Ctrl Pts',(2.61462343406994,-0.162881882998066,
-6.10622663543836E-16));
#20091=CARTESIAN_POINT('Ctrl Pts',(2.59852152905154,-0.253939094797703,
-7.38787434739808E-16));
#20092=CARTESIAN_POINT('Ctrl Pts',(2.57731092756958,-0.344277415185344,
-3.0810955291451E-16));
#20093=CARTESIAN_POINT('Ctrl Pts',(2.55115372858487,-0.433510589178544,
-3.60822483003176E-16));
#20094=CARTESIAN_POINT('Ctrl Pts',(2.54730992415644,-0.446623417870874,
-3.68568656216471E-16));
#20095=CARTESIAN_POINT('Ctrl Pts',(2.54335838534963,-0.4597150170452,-1.33461876853334E-16));
#20096=CARTESIAN_POINT('Ctrl Pts',(2.53930241226215,-0.472774949708627,
-1.38777878078145E-16));
#20097=CARTESIAN_POINT('Ctrl Pts',(2.51300579541719,-0.557448106523011,
-1.73243798916645E-16));
#20098=CARTESIAN_POINT('Ctrl Pts',(2.48237490705721,-0.640633082262047,
2.2266366763076E-16));
#20099=CARTESIAN_POINT('Ctrl Pts',(2.4476284488952,-0.722031078376524,1.66533453693773E-16));
#20100=CARTESIAN_POINT('Ctrl Pts',(2.41285997251409,-0.803480654968775,
1.10367671027941E-16));
#20101=CARTESIAN_POINT('Ctrl Pts',(2.37397005509887,-0.883141781461701,
-2.60473824643759E-16));
#20102=CARTESIAN_POINT('Ctrl Pts',(2.33113438836321,-0.960686402199183,
-2.22044604925031E-16));
#20103=CARTESIAN_POINT('Ctrl Pts',(2.28891526223189,-1.03711491080453,-1.84168503113759E-16));
#20104=CARTESIAN_POINT('Ctrl Pts',(2.24286247138705,-1.11148803969701,-4.86311355035046E-16));
#20105=CARTESIAN_POINT('Ctrl Pts',(2.19311210725222,-1.18345333925267,-6.10622663543836E-16));
#20106=CARTESIAN_POINT('Ctrl Pts',(2.16658994742807,-1.22181838863071,-6.76893623556989E-16));
#20107=CARTESIAN_POINT('Ctrl Pts',(2.13901644812981,-1.25949841963374,-1.03661145615814E-16));
#20108=CARTESIAN_POINT('Ctrl Pts',(2.11040940583919,-1.29643454206688,-5.55111512312578E-17));
#20109=CARTESIAN_POINT('Ctrl Pts',(2.10166865720486,-1.30772020237512,-4.0799144537779E-17));
#20110=CARTESIAN_POINT('Ctrl Pts',(2.09283023898332,-1.31893783850973,-3.98702450321844E-16));
#20111=CARTESIAN_POINT('Ctrl Pts',(2.08389831377262,-1.33008110200649,-3.88578058618805E-16));
#20112=CARTESIAN_POINT('Ctrl Pts',(2.03043260129099,-1.39678368942974,-3.27974347428123E-16));
#20113=CARTESIAN_POINT('Ctrl Pts',(1.97380215986925,-1.46059813131217,-2.08556400160018E-16));
#20114=CARTESIAN_POINT('Ctrl Pts',(1.91417150281915,-1.52123259912064,-1.11022302462516E-16));
#20115=CARTESIAN_POINT('Ctrl Pts',(1.85542332105702,-1.58096973622562,-1.49316138302572E-17));
#20116=CARTESIAN_POINT('Ctrl Pts',(1.79376241718216,-1.63762085789259,-5.35520206863283E-16));
#20117=CARTESIAN_POINT('Ctrl Pts',(1.72931881925135,-1.69086532717403,-5.55111512312578E-16));
#20118=CARTESIAN_POINT('Ctrl Pts',(1.66690919772329,-1.7424292882658,-5.74084474679515E-16));
#20119=CARTESIAN_POINT('Ctrl Pts',(1.60188918190129,-1.79079854027645,-4.05239810717764E-16));
#20120=CARTESIAN_POINT('Ctrl Pts',(1.53436012060039,-1.83563678794726,-4.44089209850063E-16));
#20121=CARTESIAN_POINT('Ctrl Pts',(1.48333459704145,-1.8695169429323,-4.73444140786276E-16));
#20122=CARTESIAN_POINT('Ctrl Pts',(1.43087616732457,-1.90138023485661,-2.26823314612322E-16));
#20123=CARTESIAN_POINT('Ctrl Pts',(1.37702479013106,-1.93106208855762,-2.22044604925031E-16));
#20124=CARTESIAN_POINT('Ctrl Pts',(0.260984867623806,2.92515103163649,15.058));
#20125=CARTESIAN_POINT('Ctrl Pts',(0.721611965671866,2.88493263312463,15.0330979289241));
#20126=CARTESIAN_POINT('Ctrl Pts',(1.17298362662806,2.74202417939443,15.0081958578483));
#20127=CARTESIAN_POINT('Ctrl Pts',(1.56185858228333,2.49936439089571,14.9832937867724));
#20128=CARTESIAN_POINT('Ctrl Pts',(2.3835871899963,1.98660190194863,14.930673416402));
#20129=CARTESIAN_POINT('Ctrl Pts',(2.92625811262771,1.02843390833919,14.8780530460316));
#20130=CARTESIAN_POINT('Ctrl Pts',(2.94584082398175,0.0600984948350938,
14.8254326756613));
#20131=CARTESIAN_POINT('Ctrl Pts',(2.96542353533579,-0.90823691866899,14.7728123052909));
#20132=CARTESIAN_POINT('Ctrl Pts',(2.46191803541247,-1.88673975206773,14.7201919349205));
#20133=CARTESIAN_POINT('Ctrl Pts',(1.6624759601657,-2.43293893833301,14.6675715645502));
#20134=CARTESIAN_POINT('Ctrl Pts',(0.863033884918936,-2.97913812459828,
14.6149511941798));
#20135=CARTESIAN_POINT('Ctrl Pts',(-0.232344765651281,-3.0930336637301,
14.5623308238094));
#20136=CARTESIAN_POINT('Ctrl Pts',(-1.12713695505886,-2.72269707033318,
14.5097104534391));
#20137=CARTESIAN_POINT('Ctrl Pts',(-2.02192914446644,-2.35236047693625,
14.4570900830687));
#20138=CARTESIAN_POINT('Ctrl Pts',(-2.71613487271139,-1.49779175101059,
14.4044697126983));
#20139=CARTESIAN_POINT('Ctrl Pts',(-2.89560267371491,-0.546185667602603,
14.351849342328));
#20140=CARTESIAN_POINT('Ctrl Pts',(-2.9293373183321,-0.367311836977727,
14.3419582672485));
#20141=CARTESIAN_POINT('Ctrl Pts',(-2.94488478294563,-0.185009395803266,
14.3320671921691));
#20142=CARTESIAN_POINT('Ctrl Pts',(-2.94325266537063,-0.0024318079996577,
14.3221761170896));
#20143=CARTESIAN_POINT('Origin',(0.,0.,-1.84858989190501));
#20144=CARTESIAN_POINT('',(-1.37702479013098,-1.93106208855768,0.));
#20145=CARTESIAN_POINT('Ctrl Pts',(-1.37994859234593,-1.93347131995891,
-1.03866568124111E-15));
#20146=CARTESIAN_POINT('Ctrl Pts',(-0.794305021574331,-2.34617453422284,
0.0482502273315914));
#20147=CARTESIAN_POINT('Ctrl Pts',(0.853330802601401,-2.62819893329841,
0.149165418329868));
#20148=CARTESIAN_POINT('Ctrl Pts',(2.68321992772198,-0.795544356782894,
0.30274557299483));
#20149=CARTESIAN_POINT('Ctrl Pts',(2.13222685489998,1.81318819272267,0.460740463994884));
#20150=CARTESIAN_POINT('Ctrl Pts',(-0.353356050373597,2.77617865909866,
0.618735354994938));
#20151=CARTESIAN_POINT('Ctrl Pts',(-2.12480812784407,1.50378450145058,0.74801849763165));
#20152=CARTESIAN_POINT('Ctrl Pts',(-2.36883710346974,0.358840951777969,
0.824636676601679));
#20153=CARTESIAN_POINT('Ctrl Pts',(-2.36806791026422,0.000580996437929554,
0.848589891905023));
#20154=CARTESIAN_POINT('Origin',(0.,0.,0.));
#20155=CARTESIAN_POINT('Ctrl Pts',(-1.03908919352511,2.13201587949043,-0.329233991005384));
#20156=CARTESIAN_POINT('Ctrl Pts',(-1.74458119175558,1.78817739379635,-0.2765690273387));
#20157=CARTESIAN_POINT('Ctrl Pts',(-2.77573338088225,0.351504794741619,
-0.171239100005331));
#20158=CARTESIAN_POINT('Ctrl Pts',(-1.80933791412281,-2.1375423700464,-0.013244209005277));
#20159=CARTESIAN_POINT('Ctrl Pts',(0.800729748594893,-2.68087948155196,
0.144750681994776));
#20160=CARTESIAN_POINT('Ctrl Pts',(2.68321992772198,-0.795544356782894,
0.30274557299483));
#20161=CARTESIAN_POINT('Ctrl Pts',(2.13222685489998,1.81318819272267,0.460740463994884));
#20162=CARTESIAN_POINT('Ctrl Pts',(-0.353356050373597,2.77617865909866,
0.618735354994938));
#20163=CARTESIAN_POINT('Ctrl Pts',(-2.51821971460423,1.2212058130903,0.77673024599499));
#20164=CARTESIAN_POINT('Ctrl Pts',(-2.39875016986203,-1.44183805604875,
0.934725136995045));
#20165=CARTESIAN_POINT('Ctrl Pts',(-0.103189861818606,-2.79677945469355,
1.0927200279951));
#20166=CARTESIAN_POINT('Ctrl Pts',(2.28595558559378,-1.6146683983646,1.25071491899515));
#20167=CARTESIAN_POINT('Ctrl Pts',(2.60139192527736,1.0322363870214,1.4087098099952));
#20168=CARTESIAN_POINT('Ctrl Pts',(0.556949311928898,2.7427217714679,1.56670470099526));
#20169=CARTESIAN_POINT('Ctrl Pts',(-1.99273057992189,1.96513605211958,1.72469959199531));
#20170=CARTESIAN_POINT('Ctrl Pts',(-2.73469173326279,-0.595142683011921,
1.88269448299537));
#20171=CARTESIAN_POINT('Ctrl Pts',(-0.995855715555496,-2.61553061219188,
2.04068937399542));
#20172=CARTESIAN_POINT('Ctrl Pts',(1.64637781974439,-2.26322161422709,2.19868426499547));
#20173=CARTESIAN_POINT('Ctrl Pts',(2.79508756969503,0.142186649832604,2.35667915599553));
#20174=CARTESIAN_POINT('Ctrl Pts',(1.40821242874264,2.41860884498944,2.51467404699558));
#20175=CARTESIAN_POINT('Ctrl Pts',(-1.25613315819632,2.50097199645567,2.67266893799564));
#20176=CARTESIAN_POINT('Ctrl Pts',(-2.78096812139655,0.314559449318749,
2.83066382899569));
#20177=CARTESIAN_POINT('Ctrl Pts',(-1.78302687496254,-2.15720801874703,
2.98865871999574));
#20178=CARTESIAN_POINT('Ctrl Pts',(0.832400628534772,-2.67204800324426,
3.1466536109958));
#20179=CARTESIAN_POINT('Ctrl Pts',(2.69270963387839,-0.762919488957052,
3.30464850199585));
#20180=CARTESIAN_POINT('Ctrl Pts',(2.11030679852043,1.83829718168443,3.4626433929959));
#20181=CARTESIAN_POINT('Ctrl Pts',(-0.386476751895552,2.77188871376435,
3.62063828399595));
#20182=CARTESIAN_POINT('Ctrl Pts',(-2.53266500493224,1.1909405067813,3.77863317499601));
#20183=CARTESIAN_POINT('Ctrl Pts',(-2.38132711099884,-1.47037835529628,
3.93662806599605));
#20184=CARTESIAN_POINT('Ctrl Pts',(-0.0697503817448946,-2.79783241149437,
4.09462295699612));
#20185=CARTESIAN_POINT('Ctrl Pts',(2.30510093209087,-1.58721170953314,4.25261784799616));
#20186=CARTESIAN_POINT('Ctrl Pts',(2.5888625630092,1.06326005653742,4.41061273899623));
#20187=CARTESIAN_POINT('Ctrl Pts',(0.524118009051023,2.74918744918107,4.56860762999628));
#20188=CARTESIAN_POINT('Ctrl Pts',(-2.01608414683087,1.9411687281004,4.72660252099633));
#20189=CARTESIAN_POINT('Ctrl Pts',(-2.72738037475851,-0.627795834204506,
4.88459741199638));
#20190=CARTESIAN_POINT('Ctrl Pts',(-0.964512940920624,-2.62725067416123,
5.04259230299644));
#20191=CARTESIAN_POINT('Ctrl Pts',(1.67331967629405,-2.24337526486265,5.20058719399648));
#20192=CARTESIAN_POINT('Ctrl Pts',(2.79318773824162,0.175594923072764,5.35858208499656));
#20193=CARTESIAN_POINT('Ctrl Pts',(1.37919449268132,2.43527285317938,5.51657697599659));
#20194=CARTESIAN_POINT('Ctrl Pts',(-1.28594543116668,2.48577466117395,5.67457186699666));
#20195=CARTESIAN_POINT('Ctrl Pts',(-2.78453026564846,0.281287251330417,
5.8325667579967));
#20196=CARTESIAN_POINT('Ctrl Pts',(-1.75710748413146,-2.17837200846936,
5.99056164899676));
#20197=CARTESIAN_POINT('Ctrl Pts',(0.864288593995119,-2.66190468356086,
6.14855653999681));
#20198=CARTESIAN_POINT('Ctrl Pts',(2.70163876039796,-0.730670463607777,
6.30655143099686));
#20199=CARTESIAN_POINT('Ctrl Pts',(2.08817696449889,1.86339697407977,6.46454632199692));
#20200=CARTESIAN_POINT('Ctrl Pts',(-0.419590302218696,2.76706980330411,
6.62254121299697));
#20201=CARTESIAN_POINT('Ctrl Pts',(-2.54672306405081,1.16057440653543,6.78053610399702));
#20202=CARTESIAN_POINT('Ctrl Pts',(-2.3635768050391,-1.49874480975067,6.93853099499709));
#20203=CARTESIAN_POINT('Ctrl Pts',(-0.0362940343214689,-2.79846637663312,
7.09652588599712));
#20204=CARTESIAN_POINT('Ctrl Pts',(2.32391314315961,-1.55953807940794,7.2545207769972));
#20205=CARTESIAN_POINT('Ctrl Pts',(2.57596499873257,1.09413693995685,7.41251566799723));
#20206=CARTESIAN_POINT('Ctrl Pts',(0.491210792034311,2.75525738831465,7.5705105589973));
#20207=CARTESIAN_POINT('Ctrl Pts',(-2.03914898665099,1.91692533196097,7.72850544999735));
#20208=CARTESIAN_POINT('Ctrl Pts',(-2.71967939412015,-0.66035998612245,
7.8865003409974));
#20209=CARTESIAN_POINT('Ctrl Pts',(-0.9330321424437,-2.63859476601473,8.04449523199746));
#20210=CARTESIAN_POINT('Ctrl Pts',(1.70002224901497,-2.22320841823872,8.2024901229975));
#20211=CARTESIAN_POINT('Ctrl Pts',(2.79088864512093,0.208978201275766,8.36048501399757));
#20212=CARTESIAN_POINT('Ctrl Pts',(1.34997937336987,2.45158867054595,8.51847990499762));
#20213=CARTESIAN_POINT('Ctrl Pts',(-1.31557386100644,2.47022200101732,8.67647479599767));
#20214=CARTESIAN_POINT('Ctrl Pts',(-2.78769435259396,0.247974826523285,
8.83446968699772));
#20215=CARTESIAN_POINT('Ctrl Pts',(-1.73093690286391,-2.19922458070505,
8.99246457799778));
#20216=CARTESIAN_POINT('Ctrl Pts',(0.896053003445084,-2.6513808351669,9.15045946899784));
#20217=CARTESIAN_POINT('Ctrl Pts',(2.71018167460651,-0.698316982967359,
9.30845435999788));
#20218=CARTESIAN_POINT('Ctrl Pts',(2.06574861445826,1.88823038317285,9.46644925099794));
#20219=CARTESIAN_POINT('Ctrl Pts',(-0.45264386973844,2.76185532663481,9.62444414199799));
#20220=CARTESIAN_POINT('Ctrl Pts',(-2.5604170561675,1.13004239591331,9.78243903299804));
#20221=CARTESIAN_POINT('Ctrl Pts',(-2.34548861359897,-1.52689701078686,
9.9404339239981));
#20222=CARTESIAN_POINT('Ctrl Pts',(-0.00283249851198579,-2.79870028674429,
10.0984288149982));
#20223=CARTESIAN_POINT('Ctrl Pts',(2.34239313895008,-1.53164150527581,10.2564237059982));
#20224=CARTESIAN_POINT('Ctrl Pts',(2.56269918704329,1.12485741087042,10.4144185969983));
#20225=CARTESIAN_POINT('Ctrl Pts',(0.458233353927178,2.76093344928963,10.5724134879983));
#20226=CARTESIAN_POINT('Ctrl Pts',(-2.06192231968409,1.89240790151988,10.7304083789984));
#20227=CARTESIAN_POINT('Ctrl Pts',(-2.71158962134898,-0.692829736205835,
10.8884032699984));
#20228=CARTESIAN_POINT('Ctrl Pts',(-0.90141796228012,-2.64956165719617,
11.0463981609985));
#20229=CARTESIAN_POINT('Ctrl Pts',(1.72648179491819,-2.20272375262492,11.2043930519985));
#20230=CARTESIAN_POINT('Ctrl Pts',(2.7881905800153,0.242331605070017,11.3623879429986));
#20231=CARTESIAN_POINT('Ctrl Pts',(1.32057126786748,2.46755402056041,11.5203828339987));
#20232=CARTESIAN_POINT('Ctrl Pts',(-1.34501422335496,2.45431621031658,11.6783777249987));
#20233=CARTESIAN_POINT('Ctrl Pts',(-2.79045992331823,0.214626951768239,
11.8363726159988));
#20234=CARTESIAN_POINT('Ctrl Pts',(-1.70451887724915,-2.21976276122321,
11.9943675069988));
#20235=CARTESIAN_POINT('Ctrl Pts',(0.927689321261817,-2.64047796075702,
12.1523623979988));
#20236=CARTESIAN_POINT('Ctrl Pts',(2.71833714731268,-0.66586366962402,12.3103572889989));
#20237=CARTESIAN_POINT('Ctrl Pts',(2.04302496870488,1.91279385105346,12.468352179999));
#20238=CARTESIAN_POINT('Ctrl Pts',(-0.48563275555883,2.75624604578475,12.626347070999));
#20239=CARTESIAN_POINT('Ctrl Pts',(-2.57374497374716,1.09934880708429,12.7843419619991));
#20240=CARTESIAN_POINT('Ctrl Pts',(-2.32706521767492,-1.55483087129818,
12.9423368529991));
#20241=CARTESIAN_POINT('Ctrl Pts',(0.0306296239850783,-2.7985342282319,
13.1003317439992));
#20242=CARTESIAN_POINT('Ctrl Pts',(2.36053793034993,-1.50352574600393,13.2583266349992));
#20243=CARTESIAN_POINT('Ctrl Pts',(2.54906768788899,1.15541663986578,13.4163215259993));
#20244=CARTESIAN_POINT('Ctrl Pts',(0.42518914129335,2.76621565710669,13.5743164169993));
#20245=CARTESIAN_POINT('Ctrl Pts',(-2.08439846825039,1.86761834358563,13.7323113079994));
#20246=CARTESIAN_POINT('Ctrl Pts',(-2.7031168406022,-0.725197389434075,
13.8903061989994));
#20247=CARTESIAN_POINT('Ctrl Pts',(-0.869666078203209,-2.66015561356989,
14.0483010899995));
#20248=CARTESIAN_POINT('Ctrl Pts',(1.75267763866885,-2.18191305067097,14.2062959809995));
#20249=CARTESIAN_POINT('Ctrl Pts',(2.78512620401791,0.275629071355557,14.3642908719996));
#20250=CARTESIAN_POINT('Ctrl Pts',(1.29091271455523,2.48320730756548,14.5222857629997));
#20251=CARTESIAN_POINT('Ctrl Pts',(-1.37414448785656,2.43798182357128,14.6802806539997));
#20252=CARTESIAN_POINT('Ctrl Pts',(-2.79305172314729,0.181396953694044,
14.8382755449998));
#20253=CARTESIAN_POINT('Ctrl Pts',(-1.67742675687761,-2.24026772494819,
14.9962704359998));
#20254=CARTESIAN_POINT('Ctrl Pts',(0.958368222991996,-2.62865236842956,
15.1542653269999));
#20255=CARTESIAN_POINT('Ctrl Pts',(2.7277014223945,-0.634378452891388,15.3122602179999));
#20256=CARTESIAN_POINT('Ctrl Pts',(2.01676643438217,1.93930517753648,15.470255109));
#20257=CARTESIAN_POINT('Ctrl Pts',(0.331786659212352,2.47609764328476,15.5755850363333));
#20258=CARTESIAN_POINT('Ctrl Pts',(-0.439445221994538,2.33068358199181,
15.62825));
#20259=CARTESIAN_POINT('Ctrl Pts',(-1.12236674703448,2.30288577939268,-0.219489327336923));
#20260=CARTESIAN_POINT('Ctrl Pts',(-1.88440023178909,1.93149044095738,-0.166824363670239));
#20261=CARTESIAN_POINT('Ctrl Pts',(-2.99819386511655,0.37967606197771,-0.0614944363368692));
#20262=CARTESIAN_POINT('Ctrl Pts',(-1.9543468660962,-2.30885518920509,0.096500454663184));
#20263=CARTESIAN_POINT('Ctrl Pts',(0.864904041716857,-2.89573792283723,
0.254495345663238));
#20264=CARTESIAN_POINT('Ctrl Pts',(2.89826594350265,-0.859303067925248,
0.412490236663291));
#20265=CARTESIAN_POINT('Ctrl Pts',(2.30311366337569,1.95850572434841,0.570485127663346));
#20266=CARTESIAN_POINT('Ctrl Pts',(-0.381675686047029,2.99867483004853,
0.728480018663398));
#20267=CARTESIAN_POINT('Ctrl Pts',(-2.72004182798788,1.31907905927489,0.886474909663454));
#20268=CARTESIAN_POINT('Ctrl Pts',(-2.59099742531531,-1.55739382028214,
1.0444698006635));
#20269=CARTESIAN_POINT('Ctrl Pts',(-0.111459988476451,-3.02092667145178,
1.20246469166356));
#20270=CARTESIAN_POINT('Ctrl Pts',(2.46916294621846,-1.74407560881646,1.36045958266361));
#20271=CARTESIAN_POINT('Ctrl Pts',(2.80987985548213,1.11496472400166,1.51845447366367));
#20272=CARTESIAN_POINT('Ctrl Pts',(0.60158588058462,2.96253654820512,1.67644936466372));
#20273=CARTESIAN_POINT('Ctrl Pts',(-2.15243749298894,2.12263140839256,1.83444425566377));
#20274=CARTESIAN_POINT('Ctrl Pts',(-2.95386294451934,-0.642840250207365,
1.99243914666383));
#20275=CARTESIAN_POINT('Ctrl Pts',(-1.07566833237088,-2.82515168405898,
2.15043403766388));
#20276=CARTESIAN_POINT('Ctrl Pts',(1.77832637414643,-2.44460696618424,2.30842892866393));
#20277=CARTESIAN_POINT('Ctrl Pts',(3.01909919073696,0.153582164686878,2.46642381966399));
#20278=CARTESIAN_POINT('Ctrl Pts',(1.52107327516274,2.61244766918467,2.62441871066404));
#20279=CARTESIAN_POINT('Ctrl Pts',(-1.35680564805421,2.70141179561648,2.7824136016641));
#20280=CARTESIAN_POINT('Ctrl Pts',(-3.00384814265038,0.339769740731444,
2.94040849266415));
#20281=CARTESIAN_POINT('Ctrl Pts',(-1.92592713503036,-2.33009693659115,
3.0984033836642));
#20282=CARTESIAN_POINT('Ctrl Pts',(0.899113176712534,-2.88619864782458,
3.25639827466426));
#20283=CARTESIAN_POINT('Ctrl Pts',(2.90851619987664,-0.824063487913928,
3.41439316566431));
#20284=CARTESIAN_POINT('Ctrl Pts',(2.27943682934948,1.98562706719167,3.57238805666436));
#20285=CARTESIAN_POINT('Ctrl Pts',(-0.417450838226782,2.99404106807715,
3.73038294766441));
#20286=CARTESIAN_POINT('Ctrl Pts',(-2.73564483263507,1.2863881472707,3.88837783866447));
#20287=CARTESIAN_POINT('Ctrl Pts',(-2.57217799958985,-1.5882214749488,4.04637272966452));
#20288=CARTESIAN_POINT('Ctrl Pts',(-0.0753405093145775,-3.02206401722216,
4.20436762066458));
#20289=CARTESIAN_POINT('Ctrl Pts',(2.48984269190601,-1.71441841026206,4.36236251166463));
#20290=CARTESIAN_POINT('Ctrl Pts',(2.79634633048836,1.1484747780497,4.52035740266469));
#20291=CARTESIAN_POINT('Ctrl Pts',(0.566123320833673,2.9695204161036,4.67835229366474));
#20292=CARTESIAN_POINT('Ctrl Pts',(-2.1776627259012,2.09674322895411,4.83634718466479));
#20293=CARTESIAN_POINT('Ctrl Pts',(-2.94596561894615,-0.678110380349046,
4.99434207566485));
#20294=CARTESIAN_POINT('Ctrl Pts',(-1.04181359860098,-2.83781104757613,
5.1523369666649));
#20295=CARTESIAN_POINT('Ctrl Pts',(1.80742747930962,-2.42317003592312,5.31033185766495));
#20296=CARTESIAN_POINT('Ctrl Pts',(3.01704709774863,0.189667935951029,5.46832674866501));
#20297=CARTESIAN_POINT('Ctrl Pts',(1.48972970359473,2.63044721030322,5.62632163966506));
#20298=CARTESIAN_POINT('Ctrl Pts',(-1.38900721847178,2.68499647355363,5.78431653066512));
#20299=CARTESIAN_POINT('Ctrl Pts',(-3.00769577409666,0.303830950437453,
5.94231142166516));
#20300=CARTESIAN_POINT('Ctrl Pts',(-1.89793044085485,-2.35295710917974,
6.10030631266523));
#20301=CARTESIAN_POINT('Ctrl Pts',(0.933556795495496,-2.87524239422467,
6.25830120366527));
#20302=CARTESIAN_POINT('Ctrl Pts',(2.91816094909363,-0.789229872184075,
6.41629609466533));
#20303=CARTESIAN_POINT('Ctrl Pts',(2.25553340510261,2.01273847641193,6.57429098566538));
#20304=CARTESIAN_POINT('Ctrl Pts',(-0.453218266076613,2.98883594719704,
6.73228587666544));
#20305=CARTESIAN_POINT('Ctrl Pts',(-2.75082957152067,1.25358836322381,6.89028076766548));
#20306=CARTESIAN_POINT('Ctrl Pts',(-2.55300509962799,-1.61886135207317,
7.04827565866555));
#20307=CARTESIAN_POINT('Ctrl Pts',(-0.0392028109733089,-3.02274879134448,
7.20627054966559));
#20308=CARTESIAN_POINT('Ctrl Pts',(2.51016260310644,-1.68452688370611,7.36426544066566));
#20309=CARTESIAN_POINT('Ctrl Pts',(2.78241509402469,1.18182628186475,7.5222603316657));
#20310=CARTESIAN_POINT('Ctrl Pts',(0.530578762823495,2.97607682904918,7.68025522266576));
#20311=CARTESIAN_POINT('Ctrl Pts',(-2.2025760917615,2.07055685166173,7.83825011366581));
#20312=CARTESIAN_POINT('Ctrl Pts',(-2.93764744506665,-0.713284378390626,
7.99624500466586));
#20313=CARTESIAN_POINT('Ctrl Pts',(-1.0078097791014,-2.85006430894292,8.15423989566592));
#20314=CARTESIAN_POINT('Ctrl Pts',(1.83627012329917,-2.40138692222673,8.31223478666596));
#20315=CARTESIAN_POINT('Ctrl Pts',(3.01456374436274,0.225726708956776,8.47022967766603));
#20316=CARTESIAN_POINT('Ctrl Pts',(1.45817314557243,2.64807065492862,8.62822456866608));
#20317=CARTESIAN_POINT('Ctrl Pts',(-1.42101021169528,2.66819734918923,8.78621945966612));
#20318=CARTESIAN_POINT('Ctrl Pts',(-3.01111344602942,0.267848709355943,
8.9442143506662));
#20319=CARTESIAN_POINT('Ctrl Pts',(-1.86966242464576,-2.37548090580212,
9.10220924166623));
#20320=CARTESIAN_POINT('Ctrl Pts',(0.967866955901341,-2.86387511453221,
9.26020413266631));
#20321=CARTESIAN_POINT('Ctrl Pts',(2.92738853310682,-0.754283429618888,
9.41819902366633));
#20322=CARTESIAN_POINT('Ctrl Pts',(2.23130754034209,2.03956215310421,9.57619391466641));
#20323=CARTESIAN_POINT('Ctrl Pts',(-0.488920903815691,2.98320355754919,
9.73418880566644));
#20324=CARTESIAN_POINT('Ctrl Pts',(-2.76562106534208,1.22060937195346,9.89218369666651));
#20325=CARTESIAN_POINT('Ctrl Pts',(-2.53346723443519,-1.64926980449067,
10.0501785876666));
#20326=CARTESIAN_POINT('Ctrl Pts',(-0.00305950842402692,-3.02300144812525,
10.2081734786666));
#20327=CARTESIAN_POINT('Ctrl Pts',(2.53012367371502,-1.65439454534941,10.3661683696667));
#20328=CARTESIAN_POINT('Ctrl Pts',(2.76808609704807,1.21500883753128,10.5241632606667));
#20329=CARTESIAN_POINT('Ctrl Pts',(0.494958355870487,2.98220779656589,10.6821581516668));
#20330=CARTESIAN_POINT('Ctrl Pts',(-2.22717458809345,2.0440744776545,10.8401530426668));
#20331=CARTESIAN_POINT('Ctrl Pts',(-2.92890931940236,-0.748356408785326,
10.9981479336669));
#20332=CARTESIAN_POINT('Ctrl Pts',(-0.973661888071959,-2.86191013898051,
11.1561428246669));
#20333=CARTESIAN_POINT('Ctrl Pts',(1.86485026314516,-2.37926051801397,11.314137715667));
#20334=CARTESIAN_POINT('Ctrl Pts',(3.01164944347811,0.261753213276476,11.472132606667));
#20335=CARTESIAN_POINT('Ctrl Pts',(1.42640813452734,2.66531554408024,11.6301274976671));
#20336=CARTESIAN_POINT('Ctrl Pts',(-1.45281006480367,2.6510167927182,11.7881223886671));
#20337=CARTESIAN_POINT('Ctrl Pts',(-3.01410066275426,0.231828177198969,
11.9461172796672));
#20338=CARTESIAN_POINT('Ctrl Pts',(-1.84112713272175,-2.39766511385838,
12.1041121706673));
#20339=CARTESIAN_POINT('Ctrl Pts',(1.00203875880082,-2.85209843187493,12.2621070616673));
#20340=CARTESIAN_POINT('Ctrl Pts',(2.9361976242116,-0.71922915328282,12.4201019526674));
#20341=CARTESIAN_POINT('Ctrl Pts',(2.20676271346495,2.0660942542105,12.5780968436674));
#20342=CARTESIAN_POINT('Ctrl Pts',(-0.52455367595618,2.97714472223446,12.7360917346675));
#20343=CARTESIAN_POINT('Ctrl Pts',(-2.78001714567073,1.1874558528297,12.8940866256675));
#20344=CARTESIAN_POINT('Ctrl Pts',(-2.51356729987571,-1.67944241753446,
13.0520815166676));
#20345=CARTESIAN_POINT('Ctrl Pts',(0.0330844278327718,-3.02282208089334,
13.2100764076676));
#20346=CARTESIAN_POINT('Ctrl Pts',(2.5497226750577,-1.62402545531265,13.3680712986677));
#20347=CARTESIAN_POINT('Ctrl Pts',(2.75336210467249,1.24801722858484,13.5260661896677));
#20348=CARTESIAN_POINT('Ctrl Pts',(0.459265822762407,2.98791334565805,13.6840610806678));
#20349=CARTESIAN_POINT('Ctrl Pts',(-2.25145208218098,2.01729816656161,13.8420559716679));
#20350=CARTESIAN_POINT('Ctrl Pts',(-2.91975748968037,-0.78331815979697,
14.0000508626679));
#20351=CARTESIAN_POINT('Ctrl Pts',(-0.939365256882179,-2.87335314543991,
14.158045753668));
#20352=CARTESIAN_POINT('Ctrl Pts',(1.893145566493,-2.35678194735699,14.316040644668));
#20353=CARTESIAN_POINT('Ctrl Pts',(3.0083394738034,0.297719296989276,14.4740355356681));
#20354=CARTESIAN_POINT('Ctrl Pts',(1.3943726035929,2.68222336000765,14.6320304266681));
#20355=CARTESIAN_POINT('Ctrl Pts',(-1.4842749673478,2.63337329047569,14.7900253176682));
#20356=CARTESIAN_POINT('Ctrl Pts',(-3.01690018175728,0.195934968921086,
14.9480202086682));
#20357=CARTESIAN_POINT('Ctrl Pts',(-1.81186372087882,-2.41981344296957,
15.1060150996683));
#20358=CARTESIAN_POINT('Ctrl Pts',(1.03517641373175,-2.8393250802945,15.2640099906683));
#20359=CARTESIAN_POINT('Ctrl Pts',(2.94631239686769,-0.685220561427491,
15.4220048816684));
#20360=CARTESIAN_POINT('Ctrl Pts',(2.17839969522424,2.09473032457841,15.5799997726684));
#20361=CARTESIAN_POINT('Ctrl Pts',(0.358377621218746,2.67454389339306,15.6853297000018));
#20362=CARTESIAN_POINT('Ctrl Pts',(-0.474664453622694,2.51747565713054,
15.7379946636685));
#20363=CARTESIAN_POINT('Ctrl Pts',(-1.20564430054385,2.47375567929493,-0.109744663668462));
#20364=CARTESIAN_POINT('Ctrl Pts',(-2.02421927182262,2.0748034881184,-0.057079700001777));
#20365=CARTESIAN_POINT('Ctrl Pts',(-3.22065434935084,0.407847329213798,
0.0482502273315919));
#20366=CARTESIAN_POINT('Ctrl Pts',(-2.09935581806959,-2.48016800836378,
0.206245118331646));
#20367=CARTESIAN_POINT('Ctrl Pts',(0.929078334838823,-3.11059636412251,
0.364240009331699));
#20368=CARTESIAN_POINT('Ctrl Pts',(3.11331195928332,-0.923061779067598,
0.522234900331752));
#20369=CARTESIAN_POINT('Ctrl Pts',(2.4740004718514,2.10382325597413,0.680229791331807));
#20370=CARTESIAN_POINT('Ctrl Pts',(-0.409995321720456,3.2211710009984,0.83822468233186));
#20371=CARTESIAN_POINT('Ctrl Pts',(-2.92186394137152,1.41695230545948,0.996219573331913));
#20372=CARTESIAN_POINT('Ctrl Pts',(-2.78324468076858,-1.67294958451553,
1.15421446433197));
#20373=CARTESIAN_POINT('Ctrl Pts',(-0.119730115134298,-3.24507388821001,
1.31220935533202));
#20374=CARTESIAN_POINT('Ctrl Pts',(2.65237030684314,-1.87348281926831,1.47020424633207));
#20375=CARTESIAN_POINT('Ctrl Pts',(3.0183677856869,1.19769306098192,1.62819913733213));
#20376=CARTESIAN_POINT('Ctrl Pts',(0.646222449240343,3.18235132494235,1.78619402833218));
#20377=CARTESIAN_POINT('Ctrl Pts',(-2.31214440605599,2.28012676466554,1.94418891933223));
#20378=CARTESIAN_POINT('Ctrl Pts',(-3.17303415577589,-0.690537817402807,
2.10218381033229));
#20379=CARTESIAN_POINT('Ctrl Pts',(-1.15548094918627,-3.03477275592607,
2.26017870133234));
#20380=CARTESIAN_POINT('Ctrl Pts',(1.91027492854846,-2.62599231814139,2.4181735923324));
#20381=CARTESIAN_POINT('Ctrl Pts',(3.24311081177889,0.16497767954115,2.57616848333245));
#20382=CARTESIAN_POINT('Ctrl Pts',(1.63393412158284,2.80628649337991,2.7341633743325));
#20383=CARTESIAN_POINT('Ctrl Pts',(-1.45747813791209,2.90185159477728,2.89215826533256));
#20384=CARTESIAN_POINT('Ctrl Pts',(-3.22672816390422,0.364980032144142,
3.05015315633261));
#20385=CARTESIAN_POINT('Ctrl Pts',(-2.06882739509817,-2.50298585443527,
3.20814804733266));
#20386=CARTESIAN_POINT('Ctrl Pts',(0.965825724890286,-3.10034929240489,
3.36614293833272));
#20387=CARTESIAN_POINT('Ctrl Pts',(3.1243227658749,-0.885207486870811,3.52413782933277));
#20388=CARTESIAN_POINT('Ctrl Pts',(2.44856686017853,2.13295695269892,3.68213272033283));
#20389=CARTESIAN_POINT('Ctrl Pts',(-0.448424924558006,3.21619342238995,
3.84012761133287));
#20390=CARTESIAN_POINT('Ctrl Pts',(-2.9386246603379,1.3818357877601,3.99812250233293));
#20391=CARTESIAN_POINT('Ctrl Pts',(-2.76302888818086,-1.70606459460131,
4.15611739333298));
#20392=CARTESIAN_POINT('Ctrl Pts',(-0.0809306368842651,-3.24629562294995,
4.31411228433304));
#20393=CARTESIAN_POINT('Ctrl Pts',(2.67458445172116,-1.84162511099097,4.47210717533309));
#20394=CARTESIAN_POINT('Ctrl Pts',(3.00383009796752,1.23368949956199,4.63010206633314));
#20395=CARTESIAN_POINT('Ctrl Pts',(0.608128632616327,3.18985338302612,4.7880969573332));
#20396=CARTESIAN_POINT('Ctrl Pts',(-2.33924130497153,2.25231772980782,4.94609184833325));
#20397=CARTESIAN_POINT('Ctrl Pts',(-3.16455086313379,-0.728424926493586,
5.10408673933331));
#20398=CARTESIAN_POINT('Ctrl Pts',(-1.11911425628133,-3.04837142099104,
5.26208163033336));
#20399=CARTESIAN_POINT('Ctrl Pts',(1.94153528232519,-2.60296480698359,5.42007652133342));
#20400=CARTESIAN_POINT('Ctrl Pts',(3.24090645725565,0.20374094882929,5.57807141233347));
#20401=CARTESIAN_POINT('Ctrl Pts',(1.60026491450814,2.82562156742707,5.73606630333352));
#20402=CARTESIAN_POINT('Ctrl Pts',(-1.49206900577688,2.8842182859333,5.89406119433358));
#20403=CARTESIAN_POINT('Ctrl Pts',(-3.23086128254485,0.326374649544494,
6.05205608533362));
#20404=CARTESIAN_POINT('Ctrl Pts',(-2.03875339757824,-2.52754220989012,
6.21005097633369));
#20405=CARTESIAN_POINT('Ctrl Pts',(1.00282499699587,-3.08858010488847,6.36804586733373));
#20406=CARTESIAN_POINT('Ctrl Pts',(3.1346831377893,-0.847789280760374,6.52604075833379));
#20407=CARTESIAN_POINT('Ctrl Pts',(2.42288984570632,2.16207997874408,6.68403564933384));
#20408=CARTESIAN_POINT('Ctrl Pts',(-0.486846229934527,3.21060209108997,
6.8420305403339));
#20409=CARTESIAN_POINT('Ctrl Pts',(-2.95493607899053,1.34660231991219,7.00002543133394));
#20410=CARTESIAN_POINT('Ctrl Pts',(-2.74243339421689,-1.73897789439567,
7.15802032233401));
#20411=CARTESIAN_POINT('Ctrl Pts',(-0.042111587625147,-3.24703120605584,
7.31601521333405));
#20412=CARTESIAN_POINT('Ctrl Pts',(2.69641206305327,-1.80951568800428,7.47401010433411));
#20413=CARTESIAN_POINT('Ctrl Pts',(2.98886518931682,1.26951562377266,7.63200499533417));
#20414=CARTESIAN_POINT('Ctrl Pts',(0.56994673361268,3.19689626978371,7.78999988633422));
#20415=CARTESIAN_POINT('Ctrl Pts',(-2.36600319687202,2.2241883713625,7.94799477733426));
#20416=CARTESIAN_POINT('Ctrl Pts',(-3.15561549601314,-0.766208770658805,
8.10598966833433));
#20417=CARTESIAN_POINT('Ctrl Pts',(-1.0825874157591,-3.06153385187112,8.26398455933438));
#20418=CARTESIAN_POINT('Ctrl Pts',(1.97251799758337,-2.57956542621475,8.42197945033443));
#20419=CARTESIAN_POINT('Ctrl Pts',(3.23823884360454,0.242475216637791,8.57997434133449));
#20420=CARTESIAN_POINT('Ctrl Pts',(1.566366917775,2.84455263931128,8.73796923233454));
#20421=CARTESIAN_POINT('Ctrl Pts',(-1.52644656238412,2.86617269736115,8.89596412333459));
#20422=CARTESIAN_POINT('Ctrl Pts',(-3.23453253946489,0.287722592188601,
9.05395901433465));
#20423=CARTESIAN_POINT('Ctrl Pts',(-2.0083879464276,-2.55173723089919,9.21195390533469));
#20424=CARTESIAN_POINT('Ctrl Pts',(1.0396809083576,-3.07636939389751,9.36994879633477));
#20425=CARTESIAN_POINT('Ctrl Pts',(3.14459539160713,-0.810249876270418,
9.5279436873348));
#20426=CARTESIAN_POINT('Ctrl Pts',(2.39686646622593,2.19089392303558,9.68593857833487));
#20427=CARTESIAN_POINT('Ctrl Pts',(-0.525197937892946,3.20455178846357,
9.8439334693349));
#20428=CARTESIAN_POINT('Ctrl Pts',(-2.97082507451666,1.31117634799362,10.001928360335));
#20429=CARTESIAN_POINT('Ctrl Pts',(-2.72144585527141,-1.77164259819448,
10.159923251335));
#20430=CARTESIAN_POINT('Ctrl Pts',(-0.00328651833606387,-3.24730260950622,
10.3179181423351));
#20431=CARTESIAN_POINT('Ctrl Pts',(2.71785420847995,-1.77714758542301,10.4759130333351));
#20432=CARTESIAN_POINT('Ctrl Pts',(2.97347300705285,1.30516026419214,10.6339079243352));
#20433=CARTESIAN_POINT('Ctrl Pts',(0.531683357813799,3.20348214384215,10.7919028153352));
#20434=CARTESIAN_POINT('Ctrl Pts',(-2.39242685650282,2.19574105378912,10.9498977063353));
#20435=CARTESIAN_POINT('Ctrl Pts',(-3.14622901745573,-0.803883081364814,
11.1078925973353));
#20436=CARTESIAN_POINT('Ctrl Pts',(-1.0459058138638,-3.07425862076485,11.2658874883354));
#20437=CARTESIAN_POINT('Ctrl Pts',(2.00321873137213,-2.55579728340303,11.4238823793354));
#20438=CARTESIAN_POINT('Ctrl Pts',(3.23510830694092,0.281174821482934,11.5818772703355));
#20439=CARTESIAN_POINT('Ctrl Pts',(1.5322450011872,2.86307706760007,11.7398721613356));
#20440=CARTESIAN_POINT('Ctrl Pts',(-1.56060590625239,2.84771737511982,11.8978670523356));
#20441=CARTESIAN_POINT('Ctrl Pts',(-3.23774140219028,0.2490294026297,12.0558619433357));
#20442=CARTESIAN_POINT('Ctrl Pts',(-1.97773538819436,-2.57556746649356,
12.2138568343357));
#20443=CARTESIAN_POINT('Ctrl Pts',(1.07638819633982,-3.06371890299285,12.3718517253358));
#20444=CARTESIAN_POINT('Ctrl Pts',(3.15405810111051,-0.772594636941618,
12.5298466163358));
#20445=CARTESIAN_POINT('Ctrl Pts',(2.37050045822502,2.21939465736754,12.6878415073359));
#20446=CARTESIAN_POINT('Ctrl Pts',(-0.563474596353531,3.19804339868417,
12.8458363983359));
#20447=CARTESIAN_POINT('Ctrl Pts',(-2.98628931759431,1.2755628985751,13.003831289336));
#20448=CARTESIAN_POINT('Ctrl Pts',(-2.70006938207651,-1.80405396377073,
13.161826180336));
#20449=CARTESIAN_POINT('Ctrl Pts',(0.0355392316804697,-3.24710993355476,
13.3198210713361));
#20450=CARTESIAN_POINT('Ctrl Pts',(2.73890741976546,-1.74452516462138,13.4778159623361));
#20451=CARTESIAN_POINT('Ctrl Pts',(2.95765652145599,1.3406178173039,13.6358108533362));
#20452=CARTESIAN_POINT('Ctrl Pts',(0.493342504231463,3.20961103420941,13.7938057443362));
#20453=CARTESIAN_POINT('Ctrl Pts',(-2.41850569611158,2.16697798953759,13.9518006353363));
#20454=CARTESIAN_POINT('Ctrl Pts',(-3.13639813875855,-0.841438930159867,
14.1097955263364));
#20455=CARTESIAN_POINT('Ctrl Pts',(-1.00906443556115,-3.08655067730993,
14.2677904173364));
#20456=CARTESIAN_POINT('Ctrl Pts',(2.03361349431715,-2.53165084404301,14.4257853083365));
#20457=CARTESIAN_POINT('Ctrl Pts',(3.23155274358889,0.319809522622996,14.5837801993365));
#20458=CARTESIAN_POINT('Ctrl Pts',(1.49783249263057,2.88123941244982,14.7417750903366));
#20459=CARTESIAN_POINT('Ctrl Pts',(-1.59440544683904,2.8287647573801,14.8997699813366));
#20460=CARTESIAN_POINT('Ctrl Pts',(-3.24074864036727,0.210472984148126,
15.0577648723367));
#20461=CARTESIAN_POINT('Ctrl Pts',(-1.94630068488002,-2.59935916099094,
15.2157597633367));
#20462=CARTESIAN_POINT('Ctrl Pts',(1.1119846044715,-3.04999779215944,15.3737546543368));
#20463=CARTESIAN_POINT('Ctrl Pts',(3.16492337134089,-0.73606266996359,15.5317495453368));
#20464=CARTESIAN_POINT('Ctrl Pts',(2.34003295606631,2.25015547162033,15.6897444363369));
#20465=CARTESIAN_POINT('Ctrl Pts',(0.384968583225142,2.87299014350137,15.7950743636703));
#20466=CARTESIAN_POINT('Ctrl Pts',(-0.50988368525085,2.70426773226927,15.847739327337));
#20467=CARTESIAN_POINT('Ctrl Pts',(-1.28892185405322,2.64462557919718,-2.77555756156289E-16));
#20468=CARTESIAN_POINT('Ctrl Pts',(-2.16403831185614,2.21811653527943,0.0526649636666843));
#20469=CARTESIAN_POINT('Ctrl Pts',(-3.44311483358514,0.436018596449888,
0.157994891000053));
#20470=CARTESIAN_POINT('Ctrl Pts',(-2.24436477004298,-2.65148082752247,
0.315989782000107));
#20471=CARTESIAN_POINT('Ctrl Pts',(0.99325262796079,-3.32545480540779,0.47398467300016));
#20472=CARTESIAN_POINT('Ctrl Pts',(3.32835797506399,-0.986820490209951,
0.631979564000214));
#20473=CARTESIAN_POINT('Ctrl Pts',(2.64488728032712,2.24914078759987,0.789974455000268));
#20474=CARTESIAN_POINT('Ctrl Pts',(-0.438314957393884,3.44366717194826,
0.947969346000321));
#20475=CARTESIAN_POINT('Ctrl Pts',(-3.12368605475517,1.51482555164407,1.10596423700038));
#20476=CARTESIAN_POINT('Ctrl Pts',(-2.97549193622185,-1.78850534874892,
1.26395912800043));
#20477=CARTESIAN_POINT('Ctrl Pts',(-0.128000241792142,-3.46922110496824,
1.42195401900048));
#20478=CARTESIAN_POINT('Ctrl Pts',(2.83557766746782,-2.00289002972017,1.57994891000054));
#20479=CARTESIAN_POINT('Ctrl Pts',(3.22685571589167,1.28042139796218,1.73794380100059));
#20480=CARTESIAN_POINT('Ctrl Pts',(0.690859017896064,3.40216610167957,1.89593869200064));
#20481=CARTESIAN_POINT('Ctrl Pts',(-2.47185131912304,2.43762212093852,2.0539335830007));
#20482=CARTESIAN_POINT('Ctrl Pts',(-3.39220536703243,-0.738235384598252,
2.21192847400075));
#20483=CARTESIAN_POINT('Ctrl Pts',(-1.23529356600166,-3.24439382779317,
2.3699233650008));
#20484=CARTESIAN_POINT('Ctrl Pts',(2.0422234829505,-2.80737767009854,2.52791825600086));
#20485=CARTESIAN_POINT('Ctrl Pts',(3.46712243282082,0.176373194395425,2.68591314700091));
#20486=CARTESIAN_POINT('Ctrl Pts',(1.74679496800295,3.00012531757514,2.84390803800096));
#20487=CARTESIAN_POINT('Ctrl Pts',(-1.55815062776997,3.10229139393809,3.00190292900102));
#20488=CARTESIAN_POINT('Ctrl Pts',(-3.44960818515806,0.390190323556838,
3.15989782000107));
#20489=CARTESIAN_POINT('Ctrl Pts',(-2.21172765516599,-2.67587477227939,
3.31789271100113));
#20490=CARTESIAN_POINT('Ctrl Pts',(1.03253827306805,-3.31449993698521,3.47588760200118));
#20491=CARTESIAN_POINT('Ctrl Pts',(3.34012933187316,-0.946351485827688,
3.63388249300123));
#20492=CARTESIAN_POINT('Ctrl Pts',(2.61769689100758,2.28028683820616,3.79187738400129));
#20493=CARTESIAN_POINT('Ctrl Pts',(-0.479399010889233,3.43834577670275,
3.94987227500134));
#20494=CARTESIAN_POINT('Ctrl Pts',(-3.14160448804072,1.4772834282495,4.1078671660014));
#20495=CARTESIAN_POINT('Ctrl Pts',(-2.95387977677187,-1.82390771425382,
4.26586205700145));
#20496=CARTESIAN_POINT('Ctrl Pts',(-0.0865207644539496,-3.47052722867774,
4.4238569480015));
#20497=CARTESIAN_POINT('Ctrl Pts',(2.85932621153631,-1.96883181171989,4.58185183900155));
#20498=CARTESIAN_POINT('Ctrl Pts',(3.21131386544667,1.31890422107427,4.73984673000161));
#20499=CARTESIAN_POINT('Ctrl Pts',(0.65013394439898,3.41018634994864,4.89784162100166));
#20500=CARTESIAN_POINT('Ctrl Pts',(-2.50081988404187,2.40789223066154,5.05583651200171));
#20501=CARTESIAN_POINT('Ctrl Pts',(-3.38313610732142,-0.77873947263813,
5.21383140300178));
#20502=CARTESIAN_POINT('Ctrl Pts',(-1.19641491396169,-3.25893179440594,
5.37182629400181));
#20503=CARTESIAN_POINT('Ctrl Pts',(2.07564308534076,-2.78275957804407,5.52982118500188));
#20504=CARTESIAN_POINT('Ctrl Pts',(3.46476581676266,0.217813961707557,5.68781607600192));
#20505=CARTESIAN_POINT('Ctrl Pts',(1.71080012542156,3.02079592455092,5.84581096700199));
#20506=CARTESIAN_POINT('Ctrl Pts',(-1.59513079308199,3.08344009831299,6.00380585800203));
#20507=CARTESIAN_POINT('Ctrl Pts',(-3.45402679099304,0.348918348651528,
6.1618007490021));
#20508=CARTESIAN_POINT('Ctrl Pts',(-2.17957635430163,-2.7021273106005,6.31979564000214));
#20509=CARTESIAN_POINT('Ctrl Pts',(1.07209319849625,-3.30191781555228,6.4777905310022));
#20510=CARTESIAN_POINT('Ctrl Pts',(3.35120532648497,-0.906348689336672,
6.63578542200224));
#20511=CARTESIAN_POINT('Ctrl Pts',(2.59024628631004,2.31142148107623,6.79378031300231));
#20512=CARTESIAN_POINT('Ctrl Pts',(-0.520474193792445,3.4323682349829,6.95177520400236));
#20513=CARTESIAN_POINT('Ctrl Pts',(-3.15904258646038,1.43961627660056,7.10977009500241));
#20514=CARTESIAN_POINT('Ctrl Pts',(-2.93186168880579,-1.85909443671817,
7.26776498600247));
#20515=CARTESIAN_POINT('Ctrl Pts',(-0.0450203642769841,-3.47131362076721,
7.42575987700253));
#20516=CARTESIAN_POINT('Ctrl Pts',(2.8826615230001,-1.93450449230244,7.58375476800256));
#20517=CARTESIAN_POINT('Ctrl Pts',(3.19531528460895,1.35720496568057,7.74174965900264));
#20518=CARTESIAN_POINT('Ctrl Pts',(0.609314704401862,3.41771571051825,7.89974455000267));
#20519=CARTESIAN_POINT('Ctrl Pts',(-2.52943030198254,2.37781989106326,8.05773944100274));
#20520=CARTESIAN_POINT('Ctrl Pts',(-3.37358354695964,-0.819133162926983,
8.21573433200278));
#20521=CARTESIAN_POINT('Ctrl Pts',(-1.15736505241679,-3.27300339479932,
8.37372922300284));
#20522=CARTESIAN_POINT('Ctrl Pts',(2.10876587186757,-2.75774393020277,8.53172411400289));
#20523=CARTESIAN_POINT('Ctrl Pts',(3.46191394284634,0.259223724318805,8.68971900500295));
#20524=CARTESIAN_POINT('Ctrl Pts',(1.67456068997757,3.04103462369395,8.847713896003));
#20525=CARTESIAN_POINT('Ctrl Pts',(-1.63188291307296,3.06414804553306,9.00570878700305));
#20526=CARTESIAN_POINT('Ctrl Pts',(-3.45795163290035,0.307596475021262,
9.16370367800311));
#20527=CARTESIAN_POINT('Ctrl Pts',(-2.14711346820945,-2.72799355599627,
9.32169856900316));
#20528=CARTESIAN_POINT('Ctrl Pts',(1.11149486081386,-3.28886367326282,9.47969346000322));
#20529=CARTESIAN_POINT('Ctrl Pts',(3.36180225010744,-0.866216322921951,
9.63768835100326));
#20530=CARTESIAN_POINT('Ctrl Pts',(2.56242539210976,2.34222569296695,9.79568324200333));
#20531=CARTESIAN_POINT('Ctrl Pts',(-0.561474971970195,3.42590001937795,
9.95367813300337));
#20532=CARTESIAN_POINT('Ctrl Pts',(-3.17602908369125,1.40174332403378,10.1116730240034));
#20533=CARTESIAN_POINT('Ctrl Pts',(-2.90942447610763,-1.8940153918983,10.2696679150035));
#20534=CARTESIAN_POINT('Ctrl Pts',(-0.0035135282481055,-3.47160377088719,
10.4276628060035));
#20535=CARTESIAN_POINT('Ctrl Pts',(2.90558474324488,-1.89990062549661,10.5856576970036));
#20536=CARTESIAN_POINT('Ctrl Pts',(3.17885991705762,1.39531169085301,10.7436525880036));
#20537=CARTESIAN_POINT('Ctrl Pts',(0.568408359757113,3.4247564911184,10.9016474790037));
#20538=CARTESIAN_POINT('Ctrl Pts',(-2.55767912491219,2.34740762992373,11.0596423700038));
#20539=CARTESIAN_POINT('Ctrl Pts',(-3.36354871550911,-0.859409753944302,
11.2176372610038));
#20540=CARTESIAN_POINT('Ctrl Pts',(-1.11814973965565,-3.2866071025492,11.3756321520039));
#20541=CARTESIAN_POINT('Ctrl Pts',(2.14158719959911,-2.73233404879208,11.5336270430039));
#20542=CARTESIAN_POINT('Ctrl Pts',(3.45856717040372,0.300596429689395,11.691621934004));
#20543=CARTESIAN_POINT('Ctrl Pts',(1.63808186784707,3.0608385911199,11.849616825004));
#20544=CARTESIAN_POINT('Ctrl Pts',(-1.66840174770112,3.04441795752144,12.0076117160041));
#20545=CARTESIAN_POINT('Ctrl Pts',(-3.46138214162631,0.266230628060431,
12.1656066070041));
#20546=CARTESIAN_POINT('Ctrl Pts',(-2.11434364366697,-2.75346981912873,
12.3236014980042));
#20547=CARTESIAN_POINT('Ctrl Pts',(1.15073763387882,-3.27533937411076,12.4815963890042));
#20548=CARTESIAN_POINT('Ctrl Pts',(3.37191857800943,-0.825960120600417,
12.6395912800043));
#20549=CARTESIAN_POINT('Ctrl Pts',(2.53423820298509,2.37269506052457,12.7975861710043));
#20550=CARTESIAN_POINT('Ctrl Pts',(-0.602395516750883,3.41894207513388,
12.9555810620044));
#20551=CARTESIAN_POINT('Ctrl Pts',(-3.19256148951789,1.3636699443205,13.1135759530045));
#20552=CARTESIAN_POINT('Ctrl Pts',(-2.8865714642773,-1.928665510007,13.2715708440045));
#20553=CARTESIAN_POINT('Ctrl Pts',(0.0379940355281645,-3.4713977862162,
13.4295657350046));
#20554=CARTESIAN_POINT('Ctrl Pts',(2.92809216447323,-1.8650248739301,13.5875606260046));
#20555=CARTESIAN_POINT('Ctrl Pts',(3.16195093823948,1.43321840602296,13.7455555170047));
#20556=CARTESIAN_POINT('Ctrl Pts',(0.527419185700519,3.43130872276077,13.9035504080047));
#20557=CARTESIAN_POINT('Ctrl Pts',(-2.58555931004217,2.31665781251357,14.0615452990048));
#20558=CARTESIAN_POINT('Ctrl Pts',(-3.35303878783672,-0.89955970052277,
14.2195401900048));
#20559=CARTESIAN_POINT('Ctrl Pts',(-1.07876361424012,-3.29974820917995,
14.3775350810049));
#20560=CARTESIAN_POINT('Ctrl Pts',(2.1740814221413,-2.70651974072904,14.5355299720049));
#20561=CARTESIAN_POINT('Ctrl Pts',(3.45476601337439,0.341899748256715,14.693524863005));
#20562=CARTESIAN_POINT('Ctrl Pts',(1.60129238166824,3.08025546489199,14.851519754005));
#20563=CARTESIAN_POINT('Ctrl Pts',(-1.70453592633028,3.02415622428451,15.0095146450051));
#20564=CARTESIAN_POINT('Ctrl Pts',(-3.46459709897726,0.225010999375169,
15.1675095360052));
#20565=CARTESIAN_POINT('Ctrl Pts',(-2.08073764888123,-2.77890487901232,
15.3255044270052));
#20566=CARTESIAN_POINT('Ctrl Pts',(1.18879279521126,-3.26067050402438,15.4834993180053));
#20567=CARTESIAN_POINT('Ctrl Pts',(3.38353434581409,-0.786904778499691,
15.6414942090053));
#20568=CARTESIAN_POINT('Ctrl Pts',(2.50166621690838,2.40558061866225,15.7994891000054));
#20569=CARTESIAN_POINT('Ctrl Pts',(0.411559545231536,3.07143639360967,15.9048190273387));
#20570=CARTESIAN_POINT('Ctrl Pts',(-0.545102916879006,2.891059807408,15.9574839910054));
#20571=CARTESIAN_POINT('Ctrl Pts',(-2.94111188951679,-0.00259486169482749,
14.1778238829104));
#20572=CARTESIAN_POINT('Ctrl Pts',(-2.94335307565858,-0.259762554464039,
14.1917293186085));
#20573=CARTESIAN_POINT('Ctrl Pts',(-2.91238767988341,-0.516399492336486,
14.2056347543067));
#20574=CARTESIAN_POINT('Ctrl Pts',(-2.84607967927153,-0.763554866459577,
14.2195401900048));
#20575=CARTESIAN_POINT('Ctrl Pts',(-2.59494706330453,-1.69962253674182,
14.2722051536715));
#20576=CARTESIAN_POINT('Ctrl Pts',(-1.83685533877235,-2.49968537296086,
14.3248701173382));
#20577=CARTESIAN_POINT('Ctrl Pts',(-0.915668637109368,-2.80084537966192,
14.3775350810049));
#20578=CARTESIAN_POINT('Ctrl Pts',(0.00551806455364026,-3.10200538636298,
14.4302000446716));
#20579=CARTESIAN_POINT('Ctrl Pts',(1.0897997433475,-2.90426256354601,14.4828650083382));
#20580=CARTESIAN_POINT('Ctrl Pts',(1.84538801461659,-2.29732123730656,14.5355299720049));
#20581=CARTESIAN_POINT('Ctrl Pts',(2.60097628588567,-1.6903799110671,14.5881949356716));
#20582=CARTESIAN_POINT('Ctrl Pts',(3.02787114963004,-0.674240081405173,
14.6408598993383));
#20583=CARTESIAN_POINT('Ctrl Pts',(2.93240630955118,0.29022245286501,14.693524863005));
#20584=CARTESIAN_POINT('Ctrl Pts',(2.83694146947232,1.25468498713517,14.7461898266717));
#20585=CARTESIAN_POINT('Ctrl Pts',(2.21911692557029,2.16747022601356,14.7988547903384));
#20586=CARTESIAN_POINT('Ctrl Pts',(1.35923326895286,2.61451297201819,14.851519754005));
#20587=CARTESIAN_POINT('Ctrl Pts',(0.499349612335403,3.06155571802283,14.9041847176717));
#20588=CARTESIAN_POINT('Ctrl Pts',(-0.602593156997484,3.04285597115367,
14.9568496813384));
#20589=CARTESIAN_POINT('Ctrl Pts',(-1.4469080704384,2.56698189356751,15.0095146450051));
#20590=CARTESIAN_POINT('Ctrl Pts',(-1.70601080500511,2.42094600950443,15.0256764300034));
#20591=CARTESIAN_POINT('Ctrl Pts',(-1.94085146734146,2.2318557880317,15.0418382150017));
#20592=CARTESIAN_POINT('Ctrl Pts',(-2.14373220034761,2.01193738948431,15.058));
#20593=CARTESIAN_POINT('Ctrl Pts',(-1.37994859234592,-1.93347131995891,
-1.83880688453542E-16));
#20594=CARTESIAN_POINT('Ctrl Pts',(-1.43831895271373,-1.90176082500493,
-1.96503831907269E-16));
#20595=CARTESIAN_POINT('Ctrl Pts',(-1.49514575458196,-1.86752259046863,
-3.60259795903682E-17));
#20596=CARTESIAN_POINT('Ctrl Pts',(-1.55024291463987,-1.83079524515745,
-1.11022302462516E-16));
#20597=CARTESIAN_POINT('Ctrl Pts',(-1.61820139003649,-1.78549464545158,
-1.89647209120044E-16));
#20598=CARTESIAN_POINT('Ctrl Pts',(-1.68352982136479,-1.73640902813589,
4.37133882625492E-17));
#20599=CARTESIAN_POINT('Ctrl Pts',(-1.74614398662112,-1.68389593204229,
2.08166817117217E-17));
#20600=CARTESIAN_POINT('Ctrl Pts',(-1.78291149355231,-1.65305984859862,
7.3715640875763E-18));
#20601=CARTESIAN_POINT('Ctrl Pts',(-1.81874277362574,-1.62104095184393,
-1.13501056944751E-16));
#20602=CARTESIAN_POINT('Ctrl Pts',(-1.85361742493061,-1.58790418430478,
-1.38777878078145E-16));
#20603=CARTESIAN_POINT('Ctrl Pts',(-1.86599100473682,-1.57614720832583,
-1.47746133009421E-16));
#20604=CARTESIAN_POINT('Ctrl Pts',(-1.87824533378606,-1.56424827137885,
6.18933070998169E-17));
#20605=CARTESIAN_POINT('Ctrl Pts',(-1.89037564784625,-1.55221386701801,
6.93889390390723E-18));
#20606=CARTESIAN_POINT('Ctrl Pts',(-1.9520612058093,-1.49101603289205,-2.72517484859507E-16));
#20607=CARTESIAN_POINT('Ctrl Pts',(-2.01038866542646,-1.42647262579372,
-5.93465220813464E-16));
#20608=CARTESIAN_POINT('Ctrl Pts',(-2.06526482907838,-1.35900295762991,
-3.95516952522712E-16));
#20609=CARTESIAN_POINT('Ctrl Pts',(-2.11328147227381,-1.29996699798658,
-2.22312217768304E-16));
#20610=CARTESIAN_POINT('Ctrl Pts',(-2.15865566139155,-1.2386893890933,-3.33360010116584E-16));
#20611=CARTESIAN_POINT('Ctrl Pts',(-2.20130818996771,-1.17541961668097,
-3.46944695195361E-16));
#20612=CARTESIAN_POINT('Ctrl Pts',(-2.22006840714514,-1.1475911452903,-3.52919760469855E-16));
#20613=CARTESIAN_POINT('Ctrl Pts',(-2.23830186692143,-1.11937693173939,
-3.24730293914024E-16));
#20614=CARTESIAN_POINT('Ctrl Pts',(-2.25600064404541,-1.09079672684346,
-3.05311331771918E-16));
#20615=CARTESIAN_POINT('Ctrl Pts',(-2.26668277274188,-1.07354709288677,
-2.93590982320615E-16));
#20616=CARTESIAN_POINT('Ctrl Pts',(-2.27717011522814,-1.05616412126237,
7.72460434588031E-17));
#20617=CARTESIAN_POINT('Ctrl Pts',(-2.28746078556243,-1.03865201740679,
1.38777878078145E-16));
#20618=CARTESIAN_POINT('Ctrl Pts',(-2.2952947631346,-1.02532057986291,1.85620211640871E-16));
#20619=CARTESIAN_POINT('Ctrl Pts',(-2.30301001735291,-1.01192234024488,
-2.74638834286083E-16));
#20620=CARTESIAN_POINT('Ctrl Pts',(-2.31060459934883,-0.99846213025753,
-2.77555756156289E-16));
#20621=CARTESIAN_POINT('Ctrl Pts',(-2.35418081118604,-0.921230103254969,
-2.94292477860916E-16));
#20622=CARTESIAN_POINT('Ctrl Pts',(-2.39380271969424,-0.841933889485626,
-3.78845217127159E-17));
#20623=CARTESIAN_POINT('Ctrl Pts',(-2.42937389319446,-0.760969916140703,
-6.93889390390723E-17));
#20624=CARTESIAN_POINT('Ctrl Pts',(-2.46720610926394,-0.674859556767564,
-1.02895900045749E-16));
#20625=CARTESIAN_POINT('Ctrl Pts',(-2.5004573035107,-0.586862180324133,
-9.42383278312778E-17));
#20626=CARTESIAN_POINT('Ctrl Pts',(-2.52897137574918,-0.497406668002497,
0.));
#20627=CARTESIAN_POINT('Ctrl Pts',(-2.55035692992803,-0.430315033761271,
7.06787458734584E-17));
#20628=CARTESIAN_POINT('Ctrl Pts',(-2.56907707912655,-0.362402071614612,
2.24154037051898E-16));
#20629=CARTESIAN_POINT('Ctrl Pts',(-2.58504714386116,-0.293835873442853,
2.77555756156289E-16));
#20630=CARTESIAN_POINT('Ctrl Pts',(-2.59702469241211,-0.242411224814034,
3.17607045484582E-16));
#20631=CARTESIAN_POINT('Ctrl Pts',(-2.60745499960513,-0.1906188874626,1.72939271916983E-16));
#20632=CARTESIAN_POINT('Ctrl Pts',(-2.61629539664834,-0.138527206391925,
1.38777878078145E-16));
#20633=CARTESIAN_POINT('Ctrl Pts',(-2.61869711284596,-0.124375191094725,
1.29497076264031E-16));
#20634=CARTESIAN_POINT('Ctrl Pts',(-2.62098183196127,-0.110198515695441,
1.70346493820844E-17));
#20635=CARTESIAN_POINT('Ctrl Pts',(-2.62314735205575,-0.0960068887486099,
2.77555756156289E-17));
#20636=CARTESIAN_POINT('Ctrl Pts',(-2.63712677206149,-0.00439346333649258,
9.69640447732094E-17));
#20637=CARTESIAN_POINT('Ctrl Pts',(-2.64610759043344,0.0876011416361361,
-2.12521409618605E-16));
#20638=CARTESIAN_POINT('Ctrl Pts',(-2.64996359474771,0.179577964648124,
-5.55111512312578E-17));
#20639=CARTESIAN_POINT('Ctrl Pts',(-2.65210628483955,0.230687302523444,
3.17357233945851E-17));
#20640=CARTESIAN_POINT('Ctrl Pts',(-2.65266584064783,0.281791760322423,
2.25858622101648E-16));
#20641=CARTESIAN_POINT('Ctrl Pts',(-2.65161463128253,0.332826444242184,
1.94289029309402E-16));
#20642=CARTESIAN_POINT('Ctrl Pts',(-2.64978728963931,0.421541220055518,
1.40408657934648E-16));
#20643=CARTESIAN_POINT('Ctrl Pts',(-2.6430958113368,0.510044886368098,1.72520161624302E-16));
#20644=CARTESIAN_POINT('Ctrl Pts',(-2.63178393076928,0.598076371345786,
1.66533453693773E-16));
#20645=CARTESIAN_POINT('Ctrl Pts',(-2.62024798910265,0.687851547937211,
1.60428163503557E-16));
#20646=CARTESIAN_POINT('Ctrl Pts',(-2.60390669120625,0.777136386959749,
-1.34425914858345E-16));
#20647=CARTESIAN_POINT('Ctrl Pts',(-2.58296460883121,0.865656938831555,
-1.11022302462516E-16));
#20648=CARTESIAN_POINT('Ctrl Pts',(-2.57869408333521,0.883708117645516,
-1.06249819877211E-16));
#20649=CARTESIAN_POINT('Ctrl Pts',(-2.57423206760738,0.901727502426255,
-4.70036822748448E-17));
#20650=CARTESIAN_POINT('Ctrl Pts',(-2.56958003501042,0.919712740461561,
-5.55111512312578E-17));
#20651=CARTESIAN_POINT('Ctrl Pts',(-2.56604635272843,0.933374320783267,
-6.19734215806574E-17));
#20652=CARTESIAN_POINT('Ctrl Pts',(-2.56240532303519,0.947007284078113,
8.26362614469453E-17));
#20653=CARTESIAN_POINT('Ctrl Pts',(-2.5586586911495,0.960608258314244,8.32667268468867E-17));
#20654=CARTESIAN_POINT('Ctrl Pts',(-2.53407091484386,1.04986648337083,8.74042409382574E-17));
#20655=CARTESIAN_POINT('Ctrl Pts',(-2.504930952964,1.13777933274063,7.81122475311754E-16));
#20656=CARTESIAN_POINT('Ctrl Pts',(-2.47152838793823,1.2240648243653,6.38378239159465E-16));
#20657=CARTESIAN_POINT('Ctrl Pts',(-2.43748524526305,1.31200505589874,4.92896525595146E-16));
#20658=CARTESIAN_POINT('Ctrl Pts',(-2.39901427145562,1.39825569878996,-4.49689980744232E-17));
#20659=CARTESIAN_POINT('Ctrl Pts',(-2.35636659634517,1.48252101187545,-5.55111512312578E-17));
#20660=CARTESIAN_POINT('Ctrl Pts',(-2.31336109209446,1.56749334086406,-6.61417567970626E-17));
#20661=CARTESIAN_POINT('Ctrl Pts',(-2.26610821171127,1.65044775809861,-5.44480906746773E-17));
#20662=CARTESIAN_POINT('Ctrl Pts',(-2.21481327415801,1.731071203515,-5.55111512312578E-17));
#20663=CARTESIAN_POINT('Ctrl Pts',(-2.18401751630642,1.77947481253834,-5.61493770883036E-17));
#20664=CARTESIAN_POINT('Ctrl Pts',(-2.15176385823466,1.82703799978858,3.67516605336294E-16));
#20665=CARTESIAN_POINT('Ctrl Pts',(-2.11808850376184,1.87368930169054,3.88578058618805E-16));
#20666=CARTESIAN_POINT('Ctrl Pts',(-2.1089145366433,1.88639822536441,3.94315699184355E-16));
#20667=CARTESIAN_POINT('Ctrl Pts',(-2.09963412322397,1.89904053530927,1.84615714870052E-16));
#20668=CARTESIAN_POINT('Ctrl Pts',(-2.09025911328956,1.91160012317952,1.66533453693773E-16));
#20669=CARTESIAN_POINT('Ctrl Pts',(-2.03145402967869,1.99038058527982,5.31118266465956E-17));
#20670=CARTESIAN_POINT('Ctrl Pts',(-1.96883756375661,2.06603912302101,4.62847422951145E-16));
#20671=CARTESIAN_POINT('Ctrl Pts',(-1.90268196527442,2.13826743811961,3.33066907387547E-16));
#20672=CARTESIAN_POINT('Ctrl Pts',(-1.83635976195865,2.21067765145044,2.0295955537029E-16));
#20673=CARTESIAN_POINT('Ctrl Pts',(-1.76648017672323,2.2796412428746,3.28001727774597E-18));
#20674=CARTESIAN_POINT('Ctrl Pts',(-1.6932675195623,2.34483179093341,0.));
#20675=CARTESIAN_POINT('Ctrl Pts',(-1.62146081066126,2.40877044429043,-3.21702906282713E-18));
#20676=CARTESIAN_POINT('Ctrl Pts',(-1.54644728359632,2.46908034426641,-8.3280583097932E-18));
#20677=CARTESIAN_POINT('Ctrl Pts',(-1.46839770082455,2.52542611967769,-5.55111512312578E-17));
#20678=CARTESIAN_POINT('Ctrl Pts',(-1.41023968234018,2.56741172077267,-9.06692532072844E-17));
#20679=CARTESIAN_POINT('Ctrl Pts',(-1.35039506896231,2.60719581243537,-1.11866688105539E-17));
#20680=CARTESIAN_POINT('Ctrl Pts',(-1.28892185405323,2.64462557919718,0.));
#20681=CARTESIAN_POINT('Origin',(0.,0.,0.));
#20682=CARTESIAN_POINT('Origin',(-1.44337567297407,-2.5,-6.));
#20683=CARTESIAN_POINT('',(-1.44337567297407,-2.5,-6.));
#20684=CARTESIAN_POINT('',(1.44337567297406,-2.5,-6.));
#20685=CARTESIAN_POINT('',(-0.721687836487033,-2.5,-6.));
#20686=CARTESIAN_POINT('',(-1.44337567297407,-2.5,-3.));
#20687=CARTESIAN_POINT('',(-1.44337567297407,-2.5,-6.));
#20688=CARTESIAN_POINT('',(1.44337567297406,-2.5,-3.));
#20689=CARTESIAN_POINT('',(-1.44337567297407,-2.5,-3.));
#20690=CARTESIAN_POINT('',(1.44337567297406,-2.5,-6.));
#20691=CARTESIAN_POINT('Origin',(-2.88675134594813,3.53525079574969E-16,
-6.));
#20692=CARTESIAN_POINT('',(-2.88675134594813,3.53525079574969E-16,-6.));
#20693=CARTESIAN_POINT('',(-2.52590742770461,-0.625,-6.));
#20694=CARTESIAN_POINT('',(-2.88675134594813,5.55111512312578E-16,-3.));
#20695=CARTESIAN_POINT('',(-2.88675134594813,3.53525079574969E-16,-6.));
#20696=CARTESIAN_POINT('',(-2.88675134594813,3.53525079574969E-16,-3.));
#20697=CARTESIAN_POINT('Origin',(-1.44337567297406,2.5,-6.));
#20698=CARTESIAN_POINT('',(-1.44337567297406,2.5,-6.));
#20699=CARTESIAN_POINT('',(-1.80421959121758,1.875,-6.));
#20700=CARTESIAN_POINT('',(-1.44337567297406,2.5,-3.));
#20701=CARTESIAN_POINT('',(-1.44337567297406,2.5,-6.));
#20702=CARTESIAN_POINT('',(-1.44337567297406,2.5,-3.));
#20703=CARTESIAN_POINT('Origin',(1.44337567297406,2.5,-6.));
#20704=CARTESIAN_POINT('',(1.44337567297406,2.5,-6.));
#20705=CARTESIAN_POINT('',(0.721687836487033,2.5,-6.));
#20706=CARTESIAN_POINT('',(1.44337567297406,2.5,-3.));
#20707=CARTESIAN_POINT('',(1.44337567297406,2.5,-6.));
#20708=CARTESIAN_POINT('',(1.44337567297406,2.5,-3.));
#20709=CARTESIAN_POINT('Origin',(2.88675134594813,0.,-6.));
#20710=CARTESIAN_POINT('',(2.88675134594813,0.,-6.));
#20711=CARTESIAN_POINT('',(2.52590742770461,0.625,-6.));
#20712=CARTESIAN_POINT('',(2.88675134594813,0.,-3.));
#20713=CARTESIAN_POINT('',(2.88675134594813,0.,-6.));
#20714=CARTESIAN_POINT('',(2.88675134594813,0.,-3.));
#20715=CARTESIAN_POINT('Origin',(1.44337567297406,-2.5,-6.));
#20716=CARTESIAN_POINT('',(1.80421959121758,-1.875,-6.));
#20717=CARTESIAN_POINT('',(1.44337567297406,-2.5,-3.));
#20718=CARTESIAN_POINT('Origin',(0.,0.,-3.));
#20719=CARTESIAN_POINT('Origin',(0.,0.,0.));
#20720=CARTESIAN_POINT('',(-5.,-6.12323399573677E-16,0.));
#20721=CARTESIAN_POINT('Origin',(0.,0.,0.));
#20722=CARTESIAN_POINT('Origin',(0.,0.,-6.));
#20723=CARTESIAN_POINT('',(-5.,-6.12323399573677E-16,-6.));
#20724=CARTESIAN_POINT('',(-5.,-6.12323399573677E-16,-6.));
#20725=CARTESIAN_POINT('Origin',(0.,0.,-6.));
#20726=CARTESIAN_POINT('Origin',(0.,0.,-6.));
#20727=CARTESIAN_POINT('Origin',(0.,0.,16.));
#20728=CARTESIAN_POINT('',(0.,0.,0.));
#20729=CARTESIAN_POINT('Origin',(0.,0.,0.));
#20730=CARTESIAN_POINT('',(-3.5,-4.28626379701574E-16,1.));
#20731=CARTESIAN_POINT('Origin',(0.,0.,1.));
#20732=CARTESIAN_POINT('',(-3.5,-4.28626379701574E-16,0.));
#20733=CARTESIAN_POINT('',(-3.5,-4.28626379701574E-16,0.));
#20734=CARTESIAN_POINT('Origin',(0.,0.,0.));
#20735=CARTESIAN_POINT('Origin',(0.,0.,0.));
#20736=CARTESIAN_POINT('',(-7.,-8.57252759403147E-16,1.));
#20737=CARTESIAN_POINT('Origin',(0.,0.,1.));
#20738=CARTESIAN_POINT('',(-7.,-8.57252759403147E-16,0.));
#20739=CARTESIAN_POINT('',(-7.,-8.57252759403147E-16,0.));
#20740=CARTESIAN_POINT('Origin',(0.,0.,0.));
#20741=CARTESIAN_POINT('Origin',(0.,0.,1.));
#20742=CARTESIAN_POINT('Origin',(0.,0.,0.));
#20743=CARTESIAN_POINT('',(0.,0.,0.));
#20744=CARTESIAN_POINT('Origin',(0.,0.,2.5));
#20745=CARTESIAN_POINT('',(-2.513631052301,-0.000262637959241863,0.387416697508025));
#20746=CARTESIAN_POINT('',(-2.5161395146468,-0.00304292125110089,0.112583302491978));
#20747=CARTESIAN_POINT('',(-2.5175,3.08304831685346E-16,2.5));
#20748=CARTESIAN_POINT('',(-1.91346599666505,1.63598720337496,0.));
#20749=CARTESIAN_POINT('Ctrl Pts',(-2.5161395146468,-0.00304292125110089,
0.112583302491978));
#20750=CARTESIAN_POINT('Ctrl Pts',(-2.51095752260429,0.58940711336228,0.0750555349946524));
#20751=CARTESIAN_POINT('Ctrl Pts',(-2.29922182808405,1.18480356030441,0.0375277674973267));
#20752=CARTESIAN_POINT('Ctrl Pts',(-1.91346599666507,1.63598720337494,7.63278329429795E-16));
#20753=CARTESIAN_POINT('',(1.9169334902101,1.63821054532066,9.12403139361656E-16));
#20754=CARTESIAN_POINT('Origin',(0.,0.,0.));
#20755=CARTESIAN_POINT('Ctrl Pts',(1.91694983752521,1.63822102714878,3.46944695195361E-16));
#20756=CARTESIAN_POINT('Ctrl Pts',(1.40805405000164,2.22926133126499,0.0494979486298783));
#20757=CARTESIAN_POINT('Ctrl Pts',(0.602342674674628,2.56946547367296,0.0989958972597568));
#20758=CARTESIAN_POINT('Ctrl Pts',(-0.175477465753492,2.51505986110806,
0.148493845889635));
#20759=CARTESIAN_POINT('Ctrl Pts',(-0.995235386765838,2.4577208574882,0.200660578729532));
#20760=CARTESIAN_POINT('Ctrl Pts',(-1.7840133645033,1.96207254741093,0.252827311569428));
#20761=CARTESIAN_POINT('Ctrl Pts',(-2.1906858971079,1.24828644590423,0.304994044409325));
#20762=CARTESIAN_POINT('Ctrl Pts',(-2.40486472497323,0.872362678473624,
0.332468262108891));
#20763=CARTESIAN_POINT('Ctrl Pts',(-2.51305801188577,0.435933487418771,
0.359942479808458));
#20764=CARTESIAN_POINT('Ctrl Pts',(-2.513631052301,-0.000262637959241863,
0.387416697508025));
#20765=CARTESIAN_POINT('Origin',(0.,0.,2.5));
#20766=CARTESIAN_POINT('',(-2.52068696412108,-0.00113551940461809,1.38741669750803));
#20767=CARTESIAN_POINT('',(-2.52025742113573,0.00144393706437333,1.11258330249198));
#20768=CARTESIAN_POINT('',(-2.5175,3.08304831685346E-16,2.5));
#20769=CARTESIAN_POINT('Ctrl Pts',(-2.52025742113573,0.00144393706437333,
1.11258330249198));
#20770=CARTESIAN_POINT('Ctrl Pts',(-2.52087167159714,0.0912295143008042,
1.10688933154059));
#20771=CARTESIAN_POINT('Ctrl Pts',(-2.51647663371758,0.180953836073687,
1.10119536058921));
#20772=CARTESIAN_POINT('Ctrl Pts',(-2.50686975205229,0.270115985573038,
1.09550138963782));
#20773=CARTESIAN_POINT('Ctrl Pts',(-2.41885391327537,1.08699722224894,1.04333465679793));
#20774=CARTESIAN_POINT('Ctrl Pts',(-1.89336817952545,1.85669104203942,0.991167923958032));
#20775=CARTESIAN_POINT('Ctrl Pts',(-1.16464801024837,2.23624073783096,0.939001191118135));
#20776=CARTESIAN_POINT('Ctrl Pts',(-0.435927840971309,2.6157904336225,0.886834458278239));
#20777=CARTESIAN_POINT('Ctrl Pts',(0.496026763832904,2.60519600541511,0.834667725438342));
#20778=CARTESIAN_POINT('Ctrl Pts',(1.21582156787348,2.20894038730756,0.782500992598446));
#20779=CARTESIAN_POINT('Ctrl Pts',(1.93561637191406,1.81268476920001,0.73033425975855));
#20780=CARTESIAN_POINT('Ctrl Pts',(2.443251375191,1.03076796119231,0.678167526918654));
#20781=CARTESIAN_POINT('Ctrl Pts',(2.51242958730335,0.212179626056957,0.626000794078758));
#20782=CARTESIAN_POINT('Ctrl Pts',(2.58160779941571,-0.606408709078402,
0.573834061238861));
#20783=CARTESIAN_POINT('Ctrl Pts',(2.21232922036347,-1.46166857134141,0.521667328398964));
#20784=CARTESIAN_POINT('Ctrl Pts',(1.56924485086725,-1.97326693907424,0.469500595559067));
#20785=CARTESIAN_POINT('Ctrl Pts',(0.926160481371042,-2.48486530680706,
0.417333862719171));
#20786=CARTESIAN_POINT('Ctrl Pts',(0.00927032143085621,-2.65280218000971,
0.365167129879276));
#20787=CARTESIAN_POINT('Ctrl Pts',(-0.772843960767751,-2.40046341131198,
0.31300039703938));
#20788=CARTESIAN_POINT('Ctrl Pts',(-1.55495824296637,-2.14812464261425,
0.260833664199484));
#20789=CARTESIAN_POINT('Ctrl Pts',(-2.2022966474234,-1.47551023201612,0.208666931359586));
#20790=CARTESIAN_POINT('Ctrl Pts',(-2.42598179621524,-0.686278012308338,
0.15650019851969));
#20791=CARTESIAN_POINT('Ctrl Pts',(-2.48875205155903,-0.464804623376722,
0.141861233177119));
#20792=CARTESIAN_POINT('Ctrl Pts',(-2.51816092457802,-0.234147943006738,
0.127222267834549));
#20793=CARTESIAN_POINT('Ctrl Pts',(-2.5161395146468,-0.00304292125110089,
0.112583302491978));
#20794=CARTESIAN_POINT('Ctrl Pts',(-2.513631052301,-0.000262637959241863,
0.387416697508025));
#20795=CARTESIAN_POINT('Ctrl Pts',(-2.51414607366698,-0.392294889717208,
0.412109212648355));
#20796=CARTESIAN_POINT('Ctrl Pts',(-2.42773023634316,-0.784138881365407,
0.436801727788684));
#20797=CARTESIAN_POINT('Ctrl Pts',(-2.25319678957557,-1.13170015918752,
0.461494242929014));
#20798=CARTESIAN_POINT('Ctrl Pts',(-1.88446806196691,-1.86597676983647,
0.51366097576891));
#20799=CARTESIAN_POINT('Ctrl Pts',(-1.12244351927786,-2.40260609819826,
0.565827708608806));
#20800=CARTESIAN_POINT('Ctrl Pts',(-0.306910970062746,-2.50259594233506,
0.617994441448702));
#20801=CARTESIAN_POINT('Ctrl Pts',(0.508621579152378,-2.60258578647186,
0.670161174288599));
#20802=CARTESIAN_POINT('Ctrl Pts',(1.37766213489358,-2.26593614638367,0.722327907128496));
#20803=CARTESIAN_POINT('Ctrl Pts',(1.91291169988306,-1.64259837236496,0.774494639968393));
#20804=CARTESIAN_POINT('Ctrl Pts',(2.44816126487255,-1.01926059834626,0.826661372808289));
#20805=CARTESIAN_POINT('Ctrl Pts',(2.64961983911033,-0.109234690397042,
0.878828105648185));
#20806=CARTESIAN_POINT('Ctrl Pts',(2.42745590365758,0.681791395088116,0.930994838488081));
#20807=CARTESIAN_POINT('Ctrl Pts',(2.20529196820482,1.47281748057328,0.983161571327977));
#20808=CARTESIAN_POINT('Ctrl Pts',(1.55950552306154,2.14484374359438,1.03532830416787));
#20809=CARTESIAN_POINT('Ctrl Pts',(0.777965481968195,2.39835160459691,1.08749503700777));
#20810=CARTESIAN_POINT('Ctrl Pts',(-0.00357455912515306,2.65185946559944,
1.13966176984767));
#20811=CARTESIAN_POINT('Ctrl Pts',(-0.920868196168557,2.48684892458339,
1.19182850268756));
#20812=CARTESIAN_POINT('Ctrl Pts',(-1.56505239016155,1.97685639415684,1.24399523552746));
#20813=CARTESIAN_POINT('Ctrl Pts',(-2.15540204953033,1.50948398821232,1.29180238952098));
#20814=CARTESIAN_POINT('Ctrl Pts',(-2.51638244467258,0.752380607759215,
1.3396095435145));
#20815=CARTESIAN_POINT('Ctrl Pts',(-2.52068696412108,-0.00113551940461809,
1.38741669750803));
#20816=CARTESIAN_POINT('Origin',(0.,0.,2.5));
#20817=CARTESIAN_POINT('',(-2.51584480336699,0.00196506899055149,2.38741669750802));
#20818=CARTESIAN_POINT('',(-2.51363229639634,1.41266446666228E-5,2.11258330249198));
#20819=CARTESIAN_POINT('',(-2.5175,3.08304831685346E-16,2.5));
#20820=CARTESIAN_POINT('Ctrl Pts',(-2.51363229639634,1.41266446666228E-5,
2.11258330249198));
#20821=CARTESIAN_POINT('Ctrl Pts',(-2.51365314043488,0.413200028375445,
2.08655639524664));
#20822=CARTESIAN_POINT('Ctrl Pts',(-2.41712296010665,0.826376698454607,
2.0605294880013));
#20823=CARTESIAN_POINT('Ctrl Pts',(-2.22398683849327,1.18795070900901,2.03450258075596));
#20824=CARTESIAN_POINT('Ctrl Pts',(-1.83687666966046,1.91266742746658,1.98233584791606));
#20825=CARTESIAN_POINT('Ctrl Pts',(-1.06166440870055,2.43007701911127,1.93016911507617));
#20826=CARTESIAN_POINT('Ctrl Pts',(-0.243891408049745,2.50955308940395,
1.87800238223627));
#20827=CARTESIAN_POINT('Ctrl Pts',(0.573881592601061,2.58902915969663,1.82583564939637));
#20828=CARTESIAN_POINT('Ctrl Pts',(1.43421533294277,2.23057170863728,1.77366891655648));
#20829=CARTESIAN_POINT('Ctrl Pts',(1.95362700805596,1.59395389183621,1.72150218371658));
#20830=CARTESIAN_POINT('Ctrl Pts',(2.47303868316916,0.957336075035145,1.66933545087668));
#20831=CARTESIAN_POINT('Ctrl Pts',(2.65152829305385,0.0425578924923607,
1.61716871803679));
#20832=CARTESIAN_POINT('Ctrl Pts',(2.40953581913432,-0.742620459122797,
1.56500198519689));
#20833=CARTESIAN_POINT('Ctrl Pts',(2.16754334521479,-1.52779881073796,1.51283525235699));
#20834=CARTESIAN_POINT('Ctrl Pts',(1.50506878749103,-2.1833773314255,1.4606685195171));
#20835=CARTESIAN_POINT('Ctrl Pts',(0.717402890595091,-2.41715770945467,
1.4085017866772));
#20836=CARTESIAN_POINT('Ctrl Pts',(-0.0702630063008448,-2.65093808748384,
1.35633505383731));
#20837=CARTESIAN_POINT('Ctrl Pts',(-0.983120242368966,-2.46292032285465,
1.30416832099741));
#20838=CARTESIAN_POINT('Ctrl Pts',(-1.61427588850106,-1.93687711375941,
1.25200158815751));
#20839=CARTESIAN_POINT('Ctrl Pts',(-2.17654123387562,-1.46825123921249,
1.205528826269));
#20840=CARTESIAN_POINT('Ctrl Pts',(-2.51524406302822,-0.731363410840463,
1.15905606438049));
#20841=CARTESIAN_POINT('Ctrl Pts',(-2.52025742113573,0.00144393706437333,
1.11258330249198));
#20842=CARTESIAN_POINT('Ctrl Pts',(-2.52068696412108,-0.00113551940461809,
1.38741669750803));
#20843=CARTESIAN_POINT('Ctrl Pts',(-2.52107949725397,-0.0698493560164091,
1.3917762763544));
#20844=CARTESIAN_POINT('Ctrl Pts',(-2.51850599021738,-0.138533361798365,
1.39613585520078));
#20845=CARTESIAN_POINT('Ctrl Pts',(-2.51286990332195,-0.206965106428379,
1.40049543404715));
#20846=CARTESIAN_POINT('Ctrl Pts',(-2.4454284715468,-1.02581955675002,1.45266216688705));
#20847=CARTESIAN_POINT('Ctrl Pts',(-1.93947085705393,-1.80855393755627,
1.50482889972694));
#20848=CARTESIAN_POINT('Ctrl Pts',(-1.22052386480191,-2.20627819800367,
1.55699563256684));
#20849=CARTESIAN_POINT('Ctrl Pts',(-0.501576872549894,-2.60400245845108,
1.60916236540673));
#20850=CARTESIAN_POINT('Ctrl Pts',(0.430359497461277,-2.61671659853964,
1.66132909824663));
#20851=CARTESIAN_POINT('Ctrl Pts',(1.15988750019281,-2.2387513379105,1.71349583108653));
#20852=CARTESIAN_POINT('Ctrl Pts',(1.88941550292434,-1.86078607728136,1.76566256392642));
#20853=CARTESIAN_POINT('Ctrl Pts',(2.41653513837623,-1.09214141593451,1.81782929676632));
#20854=CARTESIAN_POINT('Ctrl Pts',(2.50628871104416,-0.27543223888268,1.86999602960622));
#20855=CARTESIAN_POINT('Ctrl Pts',(2.59604228371209,0.541276938169144,1.92216276244611));
#20856=CARTESIAN_POINT('Ctrl Pts',(2.24842979359607,1.40605063092595,1.97432949528601));
#20857=CARTESIAN_POINT('Ctrl Pts',(1.61839553463159,1.93342727280644,2.02649622812591));
#20858=CARTESIAN_POINT('Ctrl Pts',(0.9883612756671,2.46080391468694,2.0786629609658));
#20859=CARTESIAN_POINT('Ctrl Pts',(0.0759052478541385,2.6507835056911,2.1308296938057));
#20860=CARTESIAN_POINT('Ctrl Pts',(-0.712256806761665,2.41868475685738,
2.1829964266456));
#20861=CARTESIAN_POINT('Ctrl Pts',(-1.50041886137746,2.18658600802365,2.23516315948549));
#20862=CARTESIAN_POINT('Ctrl Pts',(-2.16428694279611,1.53240891935204,2.28732989232539));
#20863=CARTESIAN_POINT('Ctrl Pts',(-2.40795002197348,0.747744850575128,
2.33949662516528));
#20864=CARTESIAN_POINT('Ctrl Pts',(-2.48255920772454,0.507482158922327,
2.35546998261286));
#20865=CARTESIAN_POINT('Ctrl Pts',(-2.51777110227279,0.254985358855856,
2.37144334006044));
#20866=CARTESIAN_POINT('Ctrl Pts',(-2.51584480336699,0.00196506899055149,
2.38741669750802));
#20867=CARTESIAN_POINT('Origin',(0.,0.,2.5));
#20868=CARTESIAN_POINT('',(-2.51589013302272,-0.00197902614912163,3.38741669750803));
#20869=CARTESIAN_POINT('',(-2.52021651143941,-0.00144364612508765,3.11258330249198));
#20870=CARTESIAN_POINT('',(-2.5175,3.08304831685346E-16,2.5));
#20871=CARTESIAN_POINT('Ctrl Pts',(-2.52021651143941,-0.00144364612508765,
3.11258330249198));
#20872=CARTESIAN_POINT('Ctrl Pts',(-2.51515411267109,0.729619079365268,
3.06622345895268));
#20873=CARTESIAN_POINT('Ctrl Pts',(-2.17829775808437,1.46475479323487,3.01986361541339));
#20874=CARTESIAN_POINT('Ctrl Pts',(-1.61839525002992,1.93342693235859,2.97350377187409));
#20875=CARTESIAN_POINT('Ctrl Pts',(-0.988361101417928,2.4608034807813,2.9213370390342));
#20876=CARTESIAN_POINT('Ctrl Pts',(-0.0759052345218647,2.65078303997177,
2.8691703061943));
#20877=CARTESIAN_POINT('Ctrl Pts',(0.712256681486064,2.41868433245784,2.81700357335441));
#20878=CARTESIAN_POINT('Ctrl Pts',(1.50041859749399,2.18658562494391,2.76483684051451));
#20879=CARTESIAN_POINT('Ctrl Pts',(2.16428656261379,1.53240865072558,2.71267010767461));
#20880=CARTESIAN_POINT('Ctrl Pts',(2.40794959914724,0.747744719274148,2.66050337483472));
#20881=CARTESIAN_POINT('Ctrl Pts',(2.65161263568068,-0.0369192121772903,
2.60833664199482));
#20882=CARTESIAN_POINT('Ctrl Pts',(2.47507074362777,-0.952070100861841,
2.55616990915492));
#20883=CARTESIAN_POINT('Ctrl Pts',(1.95701531533631,-1.58979072079872,2.50400317631503));
#20884=CARTESIAN_POINT('Ctrl Pts',(1.43895988704484,-2.22751134073559,2.45183644347513));
#20885=CARTESIAN_POINT('Ctrl Pts',(0.579390922514817,-2.5878016919248,2.39966971063523));
#20886=CARTESIAN_POINT('Ctrl Pts',(-0.238549412870579,-2.5100671436653,
2.34750297779534));
#20887=CARTESIAN_POINT('Ctrl Pts',(-1.05648974825598,-2.4323325954058,2.29533624495544));
#20888=CARTESIAN_POINT('Ctrl Pts',(-1.83280145449676,-1.91657314769758,
2.24316951211554));
#20889=CARTESIAN_POINT('Ctrl Pts',(-2.22145326926428,-1.19268150120826,
2.19100277927565));
#20890=CARTESIAN_POINT('Ctrl Pts',(-2.41619980794843,-0.829952222250707,
2.16486295368109));
#20891=CARTESIAN_POINT('Ctrl Pts',(-2.51361136192544,-0.414964391838591,
2.13872312808653));
#20892=CARTESIAN_POINT('Ctrl Pts',(-2.51363229639634,1.41266446666228E-5,
2.11258330249198));
#20893=CARTESIAN_POINT('Ctrl Pts',(-2.51584480336699,0.00196506899055149,
2.38741669750802));
#20894=CARTESIAN_POINT('Ctrl Pts',(-2.51148008169565,-0.571343226589796,
2.42361007290034));
#20895=CARTESIAN_POINT('Ctrl Pts',(-2.31644353295754,-1.14733917999922,
2.45980344829266));
#20896=CARTESIAN_POINT('Ctrl Pts',(-1.95701565897371,-1.58979099958587,
2.49599682368498));
#20897=CARTESIAN_POINT('Ctrl Pts',(-1.43896013986049,-2.22751173208773,
2.54816355652487));
#20898=CARTESIAN_POINT('Ctrl Pts',(-0.579391024697962,-2.58780214820923,
2.60033028936477));
#20899=CARTESIAN_POINT('Ctrl Pts',(0.238549454567511,-2.51006758543924,
2.65249702220466));
#20900=CARTESIAN_POINT('Ctrl Pts',(1.05648993383299,-2.43233302266925,2.70466375504456));
#20901=CARTESIAN_POINT('Ctrl Pts',(1.83280177720141,-1.91657348100776,2.75683048788446));
#20902=CARTESIAN_POINT('Ctrl Pts',(2.22145365982248,-1.19268170883292,2.80899722072435));
#20903=CARTESIAN_POINT('Ctrl Pts',(2.61010554244356,-0.468789936658086,
2.86116395356425));
#20904=CARTESIAN_POINT('Ctrl Pts',(2.61109746431729,0.463234066030113,2.91333068640414));
#20905=CARTESIAN_POINT('Ctrl Pts',(2.22398722823793,1.18795091427809,2.96549741924404));
#20906=CARTESIAN_POINT('Ctrl Pts',(1.83687699215856,1.91266776252607,3.01766415208394));
#20907=CARTESIAN_POINT('Ctrl Pts',(1.06166459812611,2.43007745633383,3.06983088492383));
#20908=CARTESIAN_POINT('Ctrl Pts',(0.243891452474371,2.50955353617875,3.12199761776373));
#20909=CARTESIAN_POINT('Ctrl Pts',(-0.573881693177372,2.58902961602367,
3.17416435060363));
#20910=CARTESIAN_POINT('Ctrl Pts',(-1.4342155904484,2.23057208190574,3.22633108344352));
#20911=CARTESIAN_POINT('Ctrl Pts',(-1.95362735417331,1.59395416098643,3.27849781628342));
#20912=CARTESIAN_POINT('Ctrl Pts',(-2.31512049434143,1.1508894724433,3.31480411002495));
#20913=CARTESIAN_POINT('Ctrl Pts',(-2.5114814387863,0.573092447932525,3.35111040376649));
#20914=CARTESIAN_POINT('Ctrl Pts',(-2.51589013302272,-0.00197902614912163,
3.38741669750803));
#20915=CARTESIAN_POINT('Origin',(0.,0.,2.5));
#20916=CARTESIAN_POINT('',(-2.52065797473119,0.00106685237120291,4.38741669750802));
#20917=CARTESIAN_POINT('',(-2.51644348201823,0.00207613456667446,4.11258330249198));
#20918=CARTESIAN_POINT('',(-2.5175,3.08304831685346E-16,2.5));
#20919=CARTESIAN_POINT('',(1.91346599666507,1.63598720337493,5.));
#20920=CARTESIAN_POINT('Ctrl Pts',(-2.52065797473119,0.00106685237120291,
4.38741669750802));
#20921=CARTESIAN_POINT('Ctrl Pts',(-2.51627582008385,-0.750533596725348,
4.43511093315233));
#20922=CARTESIAN_POINT('Ctrl Pts',(-2.1571958584412,-1.50553160271072,4.48280516879663));
#20923=CARTESIAN_POINT('Ctrl Pts',(-1.56924561797524,-1.97326800927033,
4.53049940444093));
#20924=CARTESIAN_POINT('Ctrl Pts',(-0.926160710476491,-2.48486610557827,
4.58266613728083));
#20925=CARTESIAN_POINT('Ctrl Pts',(-0.00926858752154605,-2.65280097461769,
4.63483287012073));
#20926=CARTESIAN_POINT('Ctrl Pts',(0.772845077643461,-2.40046275794039,
4.68699960296062));
#20927=CARTESIAN_POINT('Ctrl Pts',(1.55495874280847,-2.14812454126309,4.73916633580052));
#20928=CARTESIAN_POINT('Ctrl Pts',(2.20229395018354,-1.47551323886906,4.79133306864041));
#20929=CARTESIAN_POINT('Ctrl Pts',(2.42597897401485,-0.686281044499074,
4.84349980148031));
#20930=CARTESIAN_POINT('Ctrl Pts',(2.64966399784617,0.102951149870913,4.89566653432021));
#20931=CARTESIAN_POINT('Ctrl Pts',(2.44969883813372,1.00880423621685,4.9478332671601));
#20932=CARTESIAN_POINT('Ctrl Pts',(1.91346599666506,1.63598720337495,5.));
#20933=CARTESIAN_POINT('',(-1.91693299680257,1.63821185741719,5.));
#20934=CARTESIAN_POINT('Origin',(0.,0.,5.));
#20935=CARTESIAN_POINT('Ctrl Pts',(-1.91694926235926,1.6382222944622,5.));
#20936=CARTESIAN_POINT('Ctrl Pts',(-1.40805335272935,2.22926302987767,4.95050205137012));
#20937=CARTESIAN_POINT('Ctrl Pts',(-0.602342425840394,2.56946465859549,
4.90100410274024));
#20938=CARTESIAN_POINT('Ctrl Pts',(0.175477439781852,2.51505854463557,4.85150615411036));
#20939=CARTESIAN_POINT('Ctrl Pts',(0.995235071171573,2.45771901258696,4.79933942127047));
#20940=CARTESIAN_POINT('Ctrl Pts',(1.78401295214682,1.96207240922004,4.74717268843057));
#20941=CARTESIAN_POINT('Ctrl Pts',(2.19068546260575,1.2482867574395,4.69500595559068));
#20942=CARTESIAN_POINT('Ctrl Pts',(2.59735797306467,0.534501105658956,4.64283922275078));
#20943=CARTESIAN_POINT('Ctrl Pts',(2.62192511300726,-0.397423594535204,
4.59067248991088));
#20944=CARTESIAN_POINT('Ctrl Pts',(2.25319644256834,-1.13170027426973,4.53850575707098));
#20945=CARTESIAN_POINT('Ctrl Pts',(1.88446777212942,-1.86597695400425,4.48633902423109));
#20946=CARTESIAN_POINT('Ctrl Pts',(1.12244329130898,-2.40260561327913,4.43417229139119));
#20947=CARTESIAN_POINT('Ctrl Pts',(0.306910879222839,-2.50259532036743,
4.3820055585513));
#20948=CARTESIAN_POINT('Ctrl Pts',(-0.508621532863308,-2.60258502745572,
4.3298388257114));
#20949=CARTESIAN_POINT('Ctrl Pts',(-1.37766187621516,-2.26593578235743,
4.2776720928715));
#20950=CARTESIAN_POINT('Ctrl Pts',(-1.91291133870635,-1.64259818874412,
4.22550536003161));
#20951=CARTESIAN_POINT('Ctrl Pts',(-2.29911832868587,-1.19283157963813,
4.18786467418506));
#20952=CARTESIAN_POINT('Ctrl Pts',(-2.51154433642508,-0.59380690010991,
4.15022398833852));
#20953=CARTESIAN_POINT('Ctrl Pts',(-2.51644348201823,0.00207613456667446,
4.11258330249198));
#20954=CARTESIAN_POINT('Origin',(0.,0.,7.20842344717746));
#20955=CARTESIAN_POINT('',(-3.07686640868348,0.00176283637231212,0.791576552822548));
#20956=CARTESIAN_POINT('',(-3.06877657964135,-0.000320642608852016,0.708423447177458));
#20957=CARTESIAN_POINT('',(-3.0735,2.32747228194194E-14,7.20842344717746));
#20958=CARTESIAN_POINT('',(0.793799282532827,-2.96922295374571,0.));
#20959=CARTESIAN_POINT('Ctrl Pts',(-3.06877657964135,-0.000320642608851972,
0.708423447177458));
#20960=CARTESIAN_POINT('Ctrl Pts',(-3.06807698094575,0.532211151373012,
0.680949229477891));
#20961=CARTESIAN_POINT('Ctrl Pts',(-2.68518598576605,2.07671369914706,0.601308278938428));
#20962=CARTESIAN_POINT('Ctrl Pts',(-0.25205435815242,3.60563262622145,0.469500595559067));
#20963=CARTESIAN_POINT('Ctrl Pts',(2.8638258713055,2.21030524695087,0.313000397039378));
#20964=CARTESIAN_POINT('Ctrl Pts',(3.4222759216869,-1.16283315864926,0.15650019851969));
#20965=CARTESIAN_POINT('Ctrl Pts',(1.76703113798771,-2.70903678361537,0.0521667328398966));
#20966=CARTESIAN_POINT('Ctrl Pts',(0.793799282532827,-2.96922295374571,
0.));
#20967=CARTESIAN_POINT('',(-0.795749017144049,-2.97385877393435,2.61949253457777E-15));
#20968=CARTESIAN_POINT('Origin',(0.,0.,0.));
#20969=CARTESIAN_POINT('Ctrl Pts',(-3.07686640868348,0.00176283637231189,
0.791576552822548));
#20970=CARTESIAN_POINT('Ctrl Pts',(-3.07761631882972,0.111377919445277,
0.785882581871163));
#20971=CARTESIAN_POINT('Ctrl Pts',(-3.02309142539902,1.22449894749353,0.728021878079882));
#20972=CARTESIAN_POINT('Ctrl Pts',(-1.66998478533906,3.20643252148329,0.617994441448703));
#20973=CARTESIAN_POINT('Ctrl Pts',(1.74335679702331,3.1676297706248,0.461494242929015));
#20974=CARTESIAN_POINT('Ctrl Pts',(3.60260150316633,0.3038109312067,0.304994044409326));
#20975=CARTESIAN_POINT('Ctrl Pts',(2.27315994968988,-2.77521413120327,0.151162630099654));
#20976=CARTESIAN_POINT('Ctrl Pts',(0.124975895037349,-3.21660834551288,
0.0494979486298794));
#20977=CARTESIAN_POINT('Ctrl Pts',(-0.795758164394602,-2.97388052305263,
9.44882193321117E-16));
#20978=CARTESIAN_POINT('Origin',(0.,0.,7.20842344717746));
#20979=CARTESIAN_POINT('',(-3.06877809850016,1.72465709349923E-5,1.79157655282255));
#20980=CARTESIAN_POINT('',(-3.0773908179647,-0.00138630343203515,1.70842344717746));
#20981=CARTESIAN_POINT('',(-3.0735,2.32747228194194E-14,7.20842344717746));
#20982=CARTESIAN_POINT('Ctrl Pts',(-3.0773908179647,-0.00138630343203517,
1.70842344717746));
#20983=CARTESIAN_POINT('Ctrl Pts',(-3.07213562808389,0.918546890942566,
1.66061629318394));
#20984=CARTESIAN_POINT('Ctrl Pts',(-2.15053865242723,2.85146124051564,1.56064240635052));
#20985=CARTESIAN_POINT('Ctrl Pts',(1.11551761111489,3.4389870765969,1.4085017866772));
#20986=CARTESIAN_POINT('Ctrl Pts',(3.48075054753741,0.977649178608381,1.25200158815752));
#20987=CARTESIAN_POINT('Ctrl Pts',(2.74289601575609,-2.35537719050612,1.09550138963782));
#20988=CARTESIAN_POINT('Ctrl Pts',(-0.440018957118456,-3.58837739167123,
0.939001191118136));
#20989=CARTESIAN_POINT('Ctrl Pts',(-2.74101688880118,-1.96797948390379,
0.809975210298013));
#20990=CARTESIAN_POINT('Ctrl Pts',(-3.06940534554735,-0.47893479386132,
0.733115962317788));
#20991=CARTESIAN_POINT('Ctrl Pts',(-3.06877657964135,-0.000320642608851972,
0.708423447177458));
#20992=CARTESIAN_POINT('Ctrl Pts',(-3.06877809850016,1.72465709353392E-5,
1.79157655282255));
#20993=CARTESIAN_POINT('Ctrl Pts',(-3.06880354602845,0.504456916469473,
1.76554964557721));
#20994=CARTESIAN_POINT('Ctrl Pts',(-2.71474447759704,2.01993058914264,1.68735600549197));
#20995=CARTESIAN_POINT('Ctrl Pts',(-0.349716256635896,3.59845088308181,
1.55699563256684));
#20996=CARTESIAN_POINT('Ctrl Pts',(2.8013094644448,2.28557822072128,1.40049543404715));
#20997=CARTESIAN_POINT('Ctrl Pts',(3.45503873870173,-1.0648536490447,1.24399523552746));
#20998=CARTESIAN_POINT('Ctrl Pts',(1.02868455419652,-3.46595066989846,1.08749503700777));
#20999=CARTESIAN_POINT('Ctrl Pts',(-2.1930684252685,-2.80237835053392,0.936688809439468));
#21000=CARTESIAN_POINT('Ctrl Pts',(-3.07074583027496,-0.892887961556386,
0.83804931471106));
#21001=CARTESIAN_POINT('Ctrl Pts',(-3.07686640868348,0.00176283637231189,
0.791576552822548));
#21002=CARTESIAN_POINT('Origin',(0.,0.,7.20842344717746));
#21003=CARTESIAN_POINT('',(-3.0768164639162,-0.00176248117795978,2.79157655282255));
#21004=CARTESIAN_POINT('',(-3.07147924653364,0.00239906238030041,2.70842344717746));
#21005=CARTESIAN_POINT('',(-3.0735,2.32747228194194E-14,7.20842344717746));
#21006=CARTESIAN_POINT('Ctrl Pts',(-3.07147924653364,0.00239906238030076,
2.70842344717746));
#21007=CARTESIAN_POINT('Ctrl Pts',(-3.07383097630006,0.311299900871277,
2.69245008972988));
#21008=CARTESIAN_POINT('Ctrl Pts',(-2.89044774320411,1.62630098606235,2.6243099994424));
#21009=CARTESIAN_POINT('Ctrl Pts',(-1.02130638419203,3.46815705171515,2.50400317631503));
#21010=CARTESIAN_POINT('Ctrl Pts',(2.32062044975012,2.77234500847627,2.34750297779534));
#21011=CARTESIAN_POINT('Ctrl Pts',(3.59377276955738,-0.394942313892847,
2.19100277927565));
#21012=CARTESIAN_POINT('Ctrl Pts',(1.66316438874938,-3.21015109242256,2.03450258075596));
#21013=CARTESIAN_POINT('Ctrl Pts',(-1.7501104075517,-3.16358476523821,1.87800238223627));
#21014=CARTESIAN_POINT('Ctrl Pts',(-3.03713246509983,-1.17251597915295,
1.7693093377101));
#21015=CARTESIAN_POINT('Ctrl Pts',(-3.0778700436187,-0.0852758672160755,
1.71278302602383));
#21016=CARTESIAN_POINT('Ctrl Pts',(-3.0773908179647,-0.00138630343203517,
1.70842344717746));
#21017=CARTESIAN_POINT('Ctrl Pts',(-3.0768164639162,-0.00176248117795985,
2.79157655282255));
#21018=CARTESIAN_POINT('Ctrl Pts',(-3.0706360140197,0.890758387459429,2.74521670928325));
#21019=CARTESIAN_POINT('Ctrl Pts',(-2.19661894703825,2.79816239430364,2.64669013290406));
#21020=CARTESIAN_POINT('Ctrl Pts',(1.02130620401276,3.46815644429995,2.49599682368497));
#21021=CARTESIAN_POINT('Ctrl Pts',(3.45276382958855,1.07219267437738,2.33949662516528));
#21022=CARTESIAN_POINT('Ctrl Pts',(2.8061681927767,-2.27960425476498,2.18299642664559));
#21023=CARTESIAN_POINT('Ctrl Pts',(-0.34205648942751,-3.59919002761108,
2.02649622812591));
#21024=CARTESIAN_POINT('Ctrl Pts',(-2.71249040954675,-2.02434105954679,
1.89602293685156));
#21025=CARTESIAN_POINT('Ctrl Pts',(-3.06875254056717,-0.506610946699481,
1.8177163784171));
#21026=CARTESIAN_POINT('Ctrl Pts',(-3.06877809850016,1.72465709353392E-5,
1.79157655282255));
#21027=CARTESIAN_POINT('Origin',(0.,0.,7.20842344717746));
#21028=CARTESIAN_POINT('',(-3.0722101457728,0.00253465723558749,3.79157655282255));
#21029=CARTESIAN_POINT('',(-3.07153458742615,-0.00241610203352894,3.70842344717746));
#21030=CARTESIAN_POINT('',(-3.0735,2.32747228194194E-14,7.20842344717746));
#21031=CARTESIAN_POINT('Ctrl Pts',(-3.07153458742615,-0.00241610203352869,
3.70842344717746));
#21032=CARTESIAN_POINT('Ctrl Pts',(-3.06615221533653,0.699662219948585,
3.67211715343592));
#21033=CARTESIAN_POINT('Ctrl Pts',(-2.48197069074528,2.41863106906089,3.58364412685449));
#21034=CARTESIAN_POINT('Ctrl Pts',(0.349716325434694,3.59845154159293,3.44300436743317));
#21035=CARTESIAN_POINT('Ctrl Pts',(3.18897983255535,1.70340642470933,3.28650416891347));
#21036=CARTESIAN_POINT('Ctrl Pts',(3.18534685712864,-1.71018933171035,3.13000397039378));
#21037=CARTESIAN_POINT('Ctrl Pts',(0.342056548577105,-3.59919066394061,
2.9735037718741));
#21038=CARTESIAN_POINT('Ctrl Pts',(-2.48484176394183,-2.41428958805909,
2.83297693080198));
#21039=CARTESIAN_POINT('Ctrl Pts',(-3.06615055852694,-0.697526676037249,
2.74461682256977));
#21040=CARTESIAN_POINT('Ctrl Pts',(-3.07147924653364,0.00239906238030076,
2.70842344717746));
#21041=CARTESIAN_POINT('Ctrl Pts',(-3.0722101457728,0.00253465723558725,
3.79157655282255));
#21042=CARTESIAN_POINT('Ctrl Pts',(-3.0745183487722,0.283281367407046,3.77705050582919));
#21043=CARTESIAN_POINT('Ctrl Pts',(-2.91187546114467,1.56963838731655,3.71035772599594));
#21044=CARTESIAN_POINT('Ctrl Pts',(-1.11551737463701,3.43898632522653,3.5914982133228));
#21045=CARTESIAN_POINT('Ctrl Pts',(2.24412684766706,2.83462531411003,3.43499801480311));
#21046=CARTESIAN_POINT('Ctrl Pts',(3.60321095550619,-0.296771509319279,
3.27849781628342));
#21047=CARTESIAN_POINT('Ctrl Pts',(1.75011009124083,-3.16358418358746,3.12199761776373));
#21048=CARTESIAN_POINT('Ctrl Pts',(-1.66316409145381,-3.2101505430571,2.96549741924404));
#21049=CARTESIAN_POINT('Ctrl Pts',(-3.02187071265548,-1.22888761088956,
2.85535706426364));
#21050=CARTESIAN_POINT('Ctrl Pts',(-3.07759060777944,-0.113556859393683,
2.79738344212315));
#21051=CARTESIAN_POINT('Ctrl Pts',(-3.0768164639162,-0.00176248117795985,
2.79157655282255));
#21052=CARTESIAN_POINT('Origin',(0.,0.,7.20842344717746));
#21053=CARTESIAN_POINT('',(-3.07018609065268,-0.00333738419709156,4.79157655282255));
#21054=CARTESIAN_POINT('',(-3.07735542615147,0.00130247100806778,4.70842344717746));
#21055=CARTESIAN_POINT('',(-3.0735,2.32747228194194E-14,7.20842344717746));
#21056=CARTESIAN_POINT('',(-0.793799282532885,-2.96922295374569,5.));
#21057=CARTESIAN_POINT('Ctrl Pts',(-0.793799282532885,-2.96922295374569,
5.));
#21058=CARTESIAN_POINT('Ctrl Pts',(-1.76703113798775,-2.70903678361534,
4.9478332671601));
#21059=CARTESIAN_POINT('Ctrl Pts',(-2.8692411723445,-1.67944397566504,4.87835878476762));
#21060=CARTESIAN_POINT('Ctrl Pts',(-3.07242022864685,-0.338323361726583,
4.80888430237514));
#21061=CARTESIAN_POINT('Ctrl Pts',(-3.07018609065268,-0.00333738419709143,
4.79157655282255));
#21062=CARTESIAN_POINT('',(0.795750420935782,-2.97385779503552,5.));
#21063=CARTESIAN_POINT('Origin',(0.,0.,5.));
#21064=CARTESIAN_POINT('Ctrl Pts',(0.795759619474687,-2.97387964574988,
5.));
#21065=CARTESIAN_POINT('Ctrl Pts',(-0.124974018843371,-3.21660711871812,
4.95050205137012));
#21066=CARTESIAN_POINT('Ctrl Pts',(-2.17865809628841,-2.79463535584754,
4.85330986709594));
#21067=CARTESIAN_POINT('Ctrl Pts',(-3.0720054550259,-0.916291960093509,
4.75611768282176));
#21068=CARTESIAN_POINT('Ctrl Pts',(-3.07735542615147,0.00130247100806802,
4.70842344717746));
#21069=CARTESIAN_POINT('Origin',(0.,0.,7.20842344717746));
#21070=CARTESIAN_POINT('Ctrl Pts',(-3.07735542615147,0.00130247100806811,
4.70842344717746));
#21071=CARTESIAN_POINT('Ctrl Pts',(-3.07785711635642,0.0873493163837036,
4.70395094998186));
#21072=CARTESIAN_POINT('Ctrl Pts',(-3.03598706278426,1.17657551893794,4.64731171994637));
#21073=CARTESIAN_POINT('Ctrl Pts',(-1.74335774093941,3.16762915537798,4.53850575707099));
#21074=CARTESIAN_POINT('Ctrl Pts',(1.66998541626837,3.20643379740356,4.3820055585513));
#21075=CARTESIAN_POINT('Ctrl Pts',(3.59460935228705,0.387380778120988,4.22550536003161));
#21076=CARTESIAN_POINT('Ctrl Pts',(2.31471223100892,-2.77732417593505,4.06900516151192));
#21077=CARTESIAN_POINT('Ctrl Pts',(-1.02868478492208,-3.46595142305511,
3.91250496299223));
#21078=CARTESIAN_POINT('Ctrl Pts',(-2.89215223470734,-1.62188152779685,
3.79231105821408));
#21079=CARTESIAN_POINT('Ctrl Pts',(-3.07388588181438,-0.309119687570202,
3.72428388627582));
#21080=CARTESIAN_POINT('Ctrl Pts',(-3.07153458742615,-0.00241610203352869,
3.70842344717746));
#21081=CARTESIAN_POINT('Ctrl Pts',(-3.07018609065268,-0.00333738419709143,
4.79157655282255));
#21082=CARTESIAN_POINT('Ctrl Pts',(-3.06568638497092,0.671347129621605,
4.75671756953524));
#21083=CARTESIAN_POINT('Ctrl Pts',(-2.51923155566346,2.36462266851063,4.66969185340803));
#21084=CARTESIAN_POINT('Ctrl Pts',(0.252054090990421,3.60562829022214,4.53049940444094));
#21085=CARTESIAN_POINT('Ctrl Pts',(3.14100203598835,1.79029184281612,4.37399920592124));
#21086=CARTESIAN_POINT('Ctrl Pts',(3.23098071080095,-1.62294021205589,4.21749900740156));
#21087=CARTESIAN_POINT('Ctrl Pts',(0.440018754334274,-3.58837598279832,
4.06099880888186));
#21088=CARTESIAN_POINT('Ctrl Pts',(-2.44746347564723,-2.46982179783519,
3.91902465735553));
#21089=CARTESIAN_POINT('Ctrl Pts',(-3.06622900417178,-0.724951542199748,
3.82921723866909));
#21090=CARTESIAN_POINT('Ctrl Pts',(-3.0722101457728,0.00253465723558725,
3.79157655282255));
#21091=CARTESIAN_POINT('Ctrl Pts',(1.91346599666506,1.63598720337495,5.));
#21092=CARTESIAN_POINT('Ctrl Pts',(2.44969883813372,1.00880423621685,4.9478332671601));
#21093=CARTESIAN_POINT('Ctrl Pts',(2.84962915755861,-0.802901936475035,
4.84349980148031));
#21094=CARTESIAN_POINT('Ctrl Pts',(0.907623535433406,-2.82073584365711,
4.68699960296062));
#21095=CARTESIAN_POINT('Ctrl Pts',(-1.84305283343144,-2.31693123653885,
4.53049940444093));
#21096=CARTESIAN_POINT('Ctrl Pts',(-2.95088590955911,0.248852734190564,
4.37399920592124));
#21097=CARTESIAN_POINT('Ctrl Pts',(-1.42798214179762,2.59460107325983,4.21749900740156));
#21098=CARTESIAN_POINT('Ctrl Pts',(1.36788296256894,2.62638590693459,4.06099880888186));
#21099=CARTESIAN_POINT('Ctrl Pts',(2.94434001769405,0.317303110108862,3.90449861036218));
#21100=CARTESIAN_POINT('Ctrl Pts',(1.89597788891003,-2.27490275351114,3.74799841184249));
#21101=CARTESIAN_POINT('Ctrl Pts',(-0.842594418754297,-2.8389564690227,
3.5914982133228));
#21102=CARTESIAN_POINT('Ctrl Pts',(-2.83001837825583,-0.872220375374214,
3.43499801480311));
#21103=CARTESIAN_POINT('Ctrl Pts',(-2.29454948771943,1.8721145477878,3.27849781628342));
#21104=CARTESIAN_POINT('Ctrl Pts',(0.286452204093653,2.9474871501416,3.12199761776373));
#21105=CARTESIAN_POINT('Ctrl Pts',(2.61208938619102,1.39525806871831,2.96549741924404));
#21106=CARTESIAN_POINT('Ctrl Pts',(2.60911362056983,-1.40081393934628,2.80899722072436));
#21107=CARTESIAN_POINT('Ctrl Pts',(0.280178090464571,-2.94809256433073,
2.65249702220466));
#21108=CARTESIAN_POINT('Ctrl Pts',(-2.29852925502302,-1.86722131596623,
2.49599682368498));
#21109=CARTESIAN_POINT('Ctrl Pts',(-2.82815502421476,0.878231830680435,
2.33949662516528));
#21110=CARTESIAN_POINT('Ctrl Pts',(-0.83655077995882,2.84076309669526,2.1829964266456));
#21111=CARTESIAN_POINT('Ctrl Pts',(1.90081730348005,2.27082432368278,2.02649622812591));
#21112=CARTESIAN_POINT('Ctrl Pts',(2.94365477382811,-0.323496754587683,
1.86999602960622));
#21113=CARTESIAN_POINT('Ctrl Pts',(1.36229586747244,-2.6294307386282,1.71349583108653));
#21114=CARTESIAN_POINT('Ctrl Pts',(-1.43351324256106,-2.59128831836252,
1.55699563256684));
#21115=CARTESIAN_POINT('Ctrl Pts',(-2.95138608603967,-0.243085175943775,
1.40049543404715));
#21116=CARTESIAN_POINT('Ctrl Pts',(-1.83816183321196,2.32183838356734,1.24399523552746));
#21117=CARTESIAN_POINT('Ctrl Pts',(0.913719077918246,2.81687000661548,1.08749503700777));
#21118=CARTESIAN_POINT('Ctrl Pts',(2.85107841334811,0.800791217552173,0.930994838488081));
#21119=CARTESIAN_POINT('Ctrl Pts',(2.24670269063477,-1.92928650629548,0.774494639968393));
#21120=CARTESIAN_POINT('Ctrl Pts',(-0.360418976588814,-2.93923542656005,
0.617994441448702));
#21121=CARTESIAN_POINT('Ctrl Pts',(-2.64649260465595,-1.32934744147468,
0.461494242929014));
#21122=CARTESIAN_POINT('Ctrl Pts',(-2.57279134224077,1.46642423733366,0.304994044409324));
#21123=CARTESIAN_POINT('Ctrl Pts',(-0.206457409028375,2.95336916756547,
0.148493845889635));
#21124=CARTESIAN_POINT('Ctrl Pts',(2.34575618383328,1.81045825905282,-0.00800635263005447));
#21125=CARTESIAN_POINT('Ctrl Pts',(2.80318192056183,-0.952475183634134,
-0.164506551149743));
#21126=CARTESIAN_POINT('Ctrl Pts',(1.44737299166554,-2.21896863600185,-0.268840016829536));
#21127=CARTESIAN_POINT('Ctrl Pts',(0.650199997975074,-2.43208680203508,
-0.321006749669432));
#21128=CARTESIAN_POINT('Ctrl Pts',(2.05433155034209,1.75642532122685,5.10700224988981));
#21129=CARTESIAN_POINT('Ctrl Pts',(2.63004078503903,1.08307039382514,5.05483551704991));
#21130=CARTESIAN_POINT('Ctrl Pts',(3.05941317763178,-0.862009977081469,
4.95050205137012));
#21131=CARTESIAN_POINT('Ctrl Pts',(0.974440971474582,-3.02839279553707,
4.79400185285044));
#21132=CARTESIAN_POINT('Ctrl Pts',(-1.97873471034476,-2.48749909718309,
4.63750165433074));
#21133=CARTESIAN_POINT('Ctrl Pts',(-3.16812424993844,0.26717277658844,4.48100145581105));
#21134=CARTESIAN_POINT('Ctrl Pts',(-1.53310734151155,2.78561043396588,4.32450125729137));
#21135=CARTESIAN_POINT('Ctrl Pts',(1.46858378046875,2.81973520375758,4.16800105877167));
#21136=CARTESIAN_POINT('Ctrl Pts',(3.16109646255838,0.34066233277957,4.01150086025199));
#21137=CARTESIAN_POINT('Ctrl Pts',(2.03555600294299,-2.44237656098578,3.8550006617323));
#21138=CARTESIAN_POINT('Ctrl Pts',(-0.904624540810224,-3.0479547870335,
3.69850046321261));
#21139=CARTESIAN_POINT('Ctrl Pts',(-3.03835869183547,-0.936431501320334,
3.54200026469292));
#21140=CARTESIAN_POINT('Ctrl Pts',(-2.46346964861608,2.00993589020025,3.38550006617323));
#21141=CARTESIAN_POINT('Ctrl Pts',(0.307540244540666,3.16447528062537,3.22899986765354));
#21142=CARTESIAN_POINT('Ctrl Pts',(2.8043862016458,1.49797418738198,3.07249966913385));
#21143=CARTESIAN_POINT('Ctrl Pts',(2.80119136608943,-1.50393907013431,2.91599947061416));
#21144=CARTESIAN_POINT('Ctrl Pts',(0.300804243168747,-3.16512526420069,
2.75949927209447));
#21145=CARTESIAN_POINT('Ctrl Pts',(-2.46774239845802,-2.0046824284028,2.60299907357478));
#21146=CARTESIAN_POINT('Ctrl Pts',(-3.03635816138303,0.942885507987068,
2.44649887505509));
#21147=CARTESIAN_POINT('Ctrl Pts',(-0.898135981369886,3.04989441503522,
2.28999867653541));
#21148=CARTESIAN_POINT('Ctrl Pts',(2.04075168557006,2.43799788528061,2.13349847801572));
#21149=CARTESIAN_POINT('Ctrl Pts',(3.16036077240454,-0.347311941022739,
1.97699827949603));
#21150=CARTESIAN_POINT('Ctrl Pts',(1.46258537456475,-2.82300418989299,1.82049808097634));
#21151=CARTESIAN_POINT('Ctrl Pts',(-1.53904563089127,-2.78205380065442,
1.66399788245665));
#21152=CARTESIAN_POINT('Ctrl Pts',(-3.16866124841479,-0.260980622196635,
1.50749768393696));
#21153=CARTESIAN_POINT('Ctrl Pts',(-1.9734836444355,2.49276749859725,1.35099748541727));
#21154=CARTESIAN_POINT('Ctrl Pts',(0.98098525565046,3.02424236327596,1.19449728689758));
#21155=CARTESIAN_POINT('Ctrl Pts',(3.06096912474454,0.859743871237576,1.03799708837789));
#21156=CARTESIAN_POINT('Ctrl Pts',(2.41210046567521,-2.0713167343657,0.881496889858203));
#21157=CARTESIAN_POINT('Ctrl Pts',(-0.386952303432029,-3.15561608159711,
0.724996691338513));
#21158=CARTESIAN_POINT('Ctrl Pts',(-2.84132211649822,-1.42721135110194,
0.568496492818825));
#21159=CARTESIAN_POINT('Ctrl Pts',(-2.76219511400983,1.57437946751671,0.411996294299135));
#21160=CARTESIAN_POINT('Ctrl Pts',(-0.221656392069724,3.1707903204508,0.255496095779446));
#21161=CARTESIAN_POINT('Ctrl Pts',(2.51844607965735,1.94374058835217,0.0989958972597565));
#21162=CARTESIAN_POINT('Ctrl Pts',(3.00954658760352,-1.02259450863918,-0.0575043012599319));
#21163=CARTESIAN_POINT('Ctrl Pts',(1.55392570710626,-2.38232468520636,-0.161837766939725));
#21164=CARTESIAN_POINT('Ctrl Pts',(0.698066426160992,-2.61113218593862,
-0.214004499779622));
#21165=CARTESIAN_POINT('Ctrl Pts',(2.19519710401912,1.87686343907875,5.21400449977962));
#21166=CARTESIAN_POINT('Ctrl Pts',(2.81038273194434,1.15733655143342,5.16183776693973));
#21167=CARTESIAN_POINT('Ctrl Pts',(3.26919719770494,-0.921118017687907,
5.05750430125993));
#21168=CARTESIAN_POINT('Ctrl Pts',(1.04125840751576,-3.23604974741702,4.90100410274025));
#21169=CARTESIAN_POINT('Ctrl Pts',(-2.11441658725808,-2.65806695782732,
4.74450390422055));
#21170=CARTESIAN_POINT('Ctrl Pts',(-3.38536259031776,0.285492818986313,
4.58800370570087));
#21171=CARTESIAN_POINT('Ctrl Pts',(-1.63823254122548,2.97661979467193,4.43150350718118));
#21172=CARTESIAN_POINT('Ctrl Pts',(1.56928459836856,3.01308450058056,4.27500330866148));
#21173=CARTESIAN_POINT('Ctrl Pts',(3.37785290742272,0.364021555450283,4.1185031101418));
#21174=CARTESIAN_POINT('Ctrl Pts',(2.17513411697596,-2.60985036846042,3.96200291162211));
#21175=CARTESIAN_POINT('Ctrl Pts',(-0.966654662866148,-3.25695310504431,
3.80550271310242));
#21176=CARTESIAN_POINT('Ctrl Pts',(-3.24669900541512,-1.00064262726645,
3.64900251458273));
#21177=CARTESIAN_POINT('Ctrl Pts',(-2.63238980951274,2.1477572326127,3.49250231606304));
#21178=CARTESIAN_POINT('Ctrl Pts',(0.328628284987678,3.38146341110915,3.33600211754336));
#21179=CARTESIAN_POINT('Ctrl Pts',(2.99668301710058,1.60069030604565,3.17950191902366));
#21180=CARTESIAN_POINT('Ctrl Pts',(2.99326911160904,-1.60706420092233,3.02300172050398));
#21181=CARTESIAN_POINT('Ctrl Pts',(0.321430395872926,-3.38215796407065,
2.86650152198428));
#21182=CARTESIAN_POINT('Ctrl Pts',(-2.63695554189302,-2.14214354083938,
2.71000132346459));
#21183=CARTESIAN_POINT('Ctrl Pts',(-3.24456129855131,1.0075391852937,2.55350112494491));
#21184=CARTESIAN_POINT('Ctrl Pts',(-0.959721182780959,3.25902573337519,
2.39700092642522));
#21185=CARTESIAN_POINT('Ctrl Pts',(2.18068606766009,2.60517144687844,2.24050072790553));
#21186=CARTESIAN_POINT('Ctrl Pts',(3.37706677098096,-0.371127127457793,
2.08400052938584));
#21187=CARTESIAN_POINT('Ctrl Pts',(1.56287488165706,-3.01657764115777,1.92750033086615));
#21188=CARTESIAN_POINT('Ctrl Pts',(-1.64457801922149,-2.97281928294631,
1.77100013234646));
#21189=CARTESIAN_POINT('Ctrl Pts',(-3.3859364107899,-0.278876068449496,
1.61449993382677));
#21190=CARTESIAN_POINT('Ctrl Pts',(-2.10880545565905,2.66369661362717,1.45799973530708));
#21191=CARTESIAN_POINT('Ctrl Pts',(1.04825143338267,3.23161471993643,1.30149953678739));
#21192=CARTESIAN_POINT('Ctrl Pts',(3.27085983614097,0.918696524922978,1.1449993382677));
#21193=CARTESIAN_POINT('Ctrl Pts',(2.57749824071565,-2.21334696243591,0.988499139748014));
#21194=CARTESIAN_POINT('Ctrl Pts',(-0.413485630275245,-3.37199673663417,
0.831998941228324));
#21195=CARTESIAN_POINT('Ctrl Pts',(-3.03615162834048,-1.52507526072921,
0.675498742708636));
#21196=CARTESIAN_POINT('Ctrl Pts',(-2.9515988857789,1.68233469769977,0.518998544188945));
#21197=CARTESIAN_POINT('Ctrl Pts',(-0.23685537511107,3.38821147333612,0.362498345669257));
#21198=CARTESIAN_POINT('Ctrl Pts',(2.69113597548142,2.07702291765152,0.205998147149567));
#21199=CARTESIAN_POINT('Ctrl Pts',(3.21591125464521,-1.09271383364422,0.049497948629879));
#21200=CARTESIAN_POINT('Ctrl Pts',(1.66047842254699,-2.54568073441086,-0.0548355170499141));
#21201=CARTESIAN_POINT('Ctrl Pts',(0.745932854346909,-2.79017756984216,
-0.107002249889811));
#21202=CARTESIAN_POINT('Ctrl Pts',(2.33606265769615,1.99730155693065,5.32100674966943));
#21203=CARTESIAN_POINT('Ctrl Pts',(2.99072467884965,1.23160270904171,5.26884001682954));
#21204=CARTESIAN_POINT('Ctrl Pts',(3.47898121777811,-0.980226058294341,
5.16450655114975));
#21205=CARTESIAN_POINT('Ctrl Pts',(1.10807584355693,-3.44370669929698,5.00800635263005));
#21206=CARTESIAN_POINT('Ctrl Pts',(-2.25009846417141,-2.82863481847156,
4.85150615411037));
#21207=CARTESIAN_POINT('Ctrl Pts',(-3.60260093069709,0.30381286138419,4.69500595559067));
#21208=CARTESIAN_POINT('Ctrl Pts',(-1.74335774093941,3.16762915537798,4.53850575707099));
#21209=CARTESIAN_POINT('Ctrl Pts',(1.66998541626837,3.20643379740356,4.3820055585513));
#21210=CARTESIAN_POINT('Ctrl Pts',(3.59460935228705,0.387380778120988,4.22550536003161));
#21211=CARTESIAN_POINT('Ctrl Pts',(2.31471223100892,-2.77732417593505,4.06900516151192));
#21212=CARTESIAN_POINT('Ctrl Pts',(-1.02868478492208,-3.46595142305511,
3.91250496299223));
#21213=CARTESIAN_POINT('Ctrl Pts',(-3.45503931899475,-1.06485375321257,
3.75600476447254));
#21214=CARTESIAN_POINT('Ctrl Pts',(-2.8013099704094,2.28557857502515,3.59950456595285));
#21215=CARTESIAN_POINT('Ctrl Pts',(0.349716325434694,3.59845154159293,3.44300436743317));
#21216=CARTESIAN_POINT('Ctrl Pts',(3.18897983255535,1.70340642470933,3.28650416891347));
#21217=CARTESIAN_POINT('Ctrl Pts',(3.18534685712864,-1.71018933171035,3.13000397039378));
#21218=CARTESIAN_POINT('Ctrl Pts',(0.342056548577105,-3.59919066394061,
2.9735037718741));
#21219=CARTESIAN_POINT('Ctrl Pts',(-2.80616868532801,-2.27960465327595,
2.8170035733544));
#21220=CARTESIAN_POINT('Ctrl Pts',(-3.45276443571958,1.07219286260033,2.66050337483472));
#21221=CARTESIAN_POINT('Ctrl Pts',(-1.02130638419203,3.46815705171515,2.50400317631503));
#21222=CARTESIAN_POINT('Ctrl Pts',(2.32062044975012,2.77234500847627,2.34750297779534));
#21223=CARTESIAN_POINT('Ctrl Pts',(3.59377276955738,-0.394942313892847,
2.19100277927565));
#21224=CARTESIAN_POINT('Ctrl Pts',(1.66316438874938,-3.21015109242256,2.03450258075596));
#21225=CARTESIAN_POINT('Ctrl Pts',(-1.7501104075517,-3.16358476523821,1.87800238223627));
#21226=CARTESIAN_POINT('Ctrl Pts',(-3.60321157316502,-0.296771514702359,
1.72150218371658));
#21227=CARTESIAN_POINT('Ctrl Pts',(-2.2441272668826,2.83462572865708,1.56500198519689));
#21228=CARTESIAN_POINT('Ctrl Pts',(1.11551761111489,3.4389870765969,1.4085017866772));
#21229=CARTESIAN_POINT('Ctrl Pts',(3.48075054753741,0.977649178608381,1.25200158815752));
#21230=CARTESIAN_POINT('Ctrl Pts',(2.74289601575609,-2.35537719050612,1.09550138963782));
#21231=CARTESIAN_POINT('Ctrl Pts',(-0.440018957118456,-3.58837739167123,
0.939001191118136));
#21232=CARTESIAN_POINT('Ctrl Pts',(-3.23098114018275,-1.62293917035647,
0.782500992598446));
#21233=CARTESIAN_POINT('Ctrl Pts',(-3.14100265754796,1.79028992788282,0.626000794078757));
#21234=CARTESIAN_POINT('Ctrl Pts',(-0.25205435815242,3.60563262622145,0.469500595559067));
#21235=CARTESIAN_POINT('Ctrl Pts',(2.8638258713055,2.21030524695087,0.313000397039378));
#21236=CARTESIAN_POINT('Ctrl Pts',(3.4222759216869,-1.16283315864926,0.15650019851969));
#21237=CARTESIAN_POINT('Ctrl Pts',(1.76703113798771,-2.70903678361537,0.0521667328398966));
#21238=CARTESIAN_POINT('Ctrl Pts',(0.793799282532827,-2.96922295374571,
0.));
#21239=CARTESIAN_POINT('Ctrl Pts',(0.793799282532827,-2.96922295374571,
0.));
#21240=CARTESIAN_POINT('Ctrl Pts',(0.886893769048896,-2.93516857472777,
6.49317190359092E-17));
#21241=CARTESIAN_POINT('Ctrl Pts',(0.977926242508662,-2.8963539026744,3.5899553935387E-16));
#21242=CARTESIAN_POINT('Ctrl Pts',(1.06668623690149,-2.85310458823344,2.77555756156289E-16));
#21243=CARTESIAN_POINT('Ctrl Pts',(1.1573833631875,-2.8089113842966,1.94338600140189E-16));
#21244=CARTESIAN_POINT('Ctrl Pts',(1.24570840723307,-2.76008724482105,8.94098625496742E-16));
#21245=CARTESIAN_POINT('Ctrl Pts',(1.33140791312673,-2.70693413976456,1.38777878078145E-15));
#21246=CARTESIAN_POINT('Ctrl Pts',(1.41293443628286,-2.65636922920854,1.85742007207992E-15));
#21247=CARTESIAN_POINT('Ctrl Pts',(1.49208510125195,-2.60188577643099,1.19996770961849E-15));
#21248=CARTESIAN_POINT('Ctrl Pts',(1.5686100025003,-2.54371483646266,1.16573417585641E-15));
#21249=CARTESIAN_POINT('Ctrl Pts',(1.63556929109261,-2.49281526399038,1.1357798338146E-15));
#21250=CARTESIAN_POINT('Ctrl Pts',(1.70051795047849,-2.43909179704035,4.6524848618713E-16));
#21251=CARTESIAN_POINT('Ctrl Pts',(1.7632650317936,-2.38268698713509,5.55111512312578E-16));
#21252=CARTESIAN_POINT('Ctrl Pts',(1.77895111395862,-2.36858640326518,5.7757628329248E-16));
#21253=CARTESIAN_POINT('Ctrl Pts',(1.79450367669767,-2.35431414158982,1.61759689860544E-15));
#21254=CARTESIAN_POINT('Ctrl Pts',(1.80989558143071,-2.33989519409729,1.66533453693773E-15));
#21255=CARTESIAN_POINT('Ctrl Pts',(1.88231905248557,-2.27204977506178,1.88995426581157E-15));
#21256=CARTESIAN_POINT('Ctrl Pts',(1.95127638915324,-2.2008843069976,9.33280417709878E-16));
#21257=CARTESIAN_POINT('Ctrl Pts',(2.01652605934852,-2.12668615788006,7.49400541621981E-16));
#21258=CARTESIAN_POINT('Ctrl Pts',(2.08140793958276,-2.05290623822316,5.66557133186095E-16));
#21259=CARTESIAN_POINT('Ctrl Pts',(2.14262432088329,-1.97612693884884,9.5775323130718E-16));
#21260=CARTESIAN_POINT('Ctrl Pts',(2.19989413197892,-1.89660402190249,6.93889390390723E-16));
#21261=CARTESIAN_POINT('Ctrl Pts',(2.25380415733742,-1.82174638945804,4.45505362525734E-16));
#21262=CARTESIAN_POINT('Ctrl Pts',(2.30421707668655,-1.74445688295852,3.26466360005673E-15));
#21263=CARTESIAN_POINT('Ctrl Pts',(2.35085702030783,-1.6649361419825,3.7470027081099E-15));
#21264=CARTESIAN_POINT('Ctrl Pts',(2.38695907926369,-1.60338241236736,4.12036154098178E-15));
#21265=CARTESIAN_POINT('Ctrl Pts',(2.42079974187715,-1.54049148436203,2.76023327184715E-15));
#21266=CARTESIAN_POINT('Ctrl Pts',(2.45223230030139,-1.47635450699168,2.80331313717852E-15));
#21267=CARTESIAN_POINT('Ctrl Pts',(2.45885027647649,-1.46285077043765,2.81238339861069E-15));
#21268=CARTESIAN_POINT('Ctrl Pts',(2.46536173765269,-1.4492909927482,2.25462528933555E-15));
#21269=CARTESIAN_POINT('Ctrl Pts',(2.47175843746063,-1.43569095783397,2.27595720048157E-15));
#21270=CARTESIAN_POINT('Ctrl Pts',(2.51224387039329,-1.34961480639136,2.41096926669652E-15));
#21271=CARTESIAN_POINT('Ctrl Pts',(2.5482055573203,-1.26178852463594,3.62029001511052E-15));
#21272=CARTESIAN_POINT('Ctrl Pts',(2.57938539343216,-1.17245068676435,3.44169137633799E-15));
#21273=CARTESIAN_POINT('Ctrl Pts',(2.61056522954403,-1.08311284889276,3.26309273756545E-15));
#21274=CARTESIAN_POINT('Ctrl Pts',(2.6369636677978,-0.99226274488999,1.94109001754332E-16));
#21275=CARTESIAN_POINT('Ctrl Pts',(2.65826790515113,-0.90012905980095,-3.60822483003176E-16));
#21276=CARTESIAN_POINT('Ctrl Pts',(2.67972711543533,-0.807325168734929,
-9.19790693281215E-16));
#21277=CARTESIAN_POINT('Ctrl Pts',(2.6960170532411,-0.713217781371016,2.19518166871644E-16));
#21278=CARTESIAN_POINT('Ctrl Pts',(2.70721235053312,-0.618215105888531,
0.));
#21279=CARTESIAN_POINT('Ctrl Pts',(2.71292160521868,-0.56976668544991,-1.11947462410922E-16));
#21280=CARTESIAN_POINT('Ctrl Pts',(2.71730508064361,-0.521085594130936,
7.31925815782227E-16));
#21281=CARTESIAN_POINT('Ctrl Pts',(2.72036776812806,-0.472227710003176,
7.49400541621981E-16));
#21282=CARTESIAN_POINT('Ctrl Pts',(2.72142942533794,-0.455291497866967,
7.55458021783632E-16));
#21283=CARTESIAN_POINT('Ctrl Pts',(2.72233234751915,-0.438334056241388,
1.47771822505628E-15));
#21284=CARTESIAN_POINT('Ctrl Pts',(2.72307665503345,-0.421357761541496,
1.52655665885959E-15));
#21285=CARTESIAN_POINT('Ctrl Pts',(2.72371406196817,-0.40681967377542,1.56838071113613E-15));
#21286=CARTESIAN_POINT('Ctrl Pts',(2.72423475300693,-0.392276144899293,
-5.84163957766239E-16));
#21287=CARTESIAN_POINT('Ctrl Pts',(2.72463912967391,-0.377733018449256,
-5.82867087928207E-16));
#21288=CARTESIAN_POINT('Ctrl Pts',(2.7272335888012,-0.284425094826578,-5.74546440218005E-16));
#21289=CARTESIAN_POINT('Ctrl Pts',(2.72504700910767,-0.191075061278942,
2.51838167646803E-15));
#21290=CARTESIAN_POINT('Ctrl Pts',(2.71820565462271,-0.0980605230163078,
1.9151347174784E-15));
#21291=CARTESIAN_POINT('Ctrl Pts',(2.71136113957177,-0.00500301393752514,
1.31160907071961E-15));
#21292=CARTESIAN_POINT('Ctrl Pts',(2.69985717427859,0.0877196672682859,
-3.07238256336187E-16));
#21293=CARTESIAN_POINT('Ctrl Pts',(2.68376968445062,0.179716676654276,-1.04083408558608E-15));
#21294=CARTESIAN_POINT('Ctrl Pts',(2.6679263547778,0.270317445587206,-1.76329611625024E-15));
#21295=CARTESIAN_POINT('Ctrl Pts',(2.64763712143603,0.360215237891958,2.87404250511705E-16));
#21296=CARTESIAN_POINT('Ctrl Pts',(2.62293183221363,0.449011051883673,-1.38777878078145E-17));
#21297=CARTESIAN_POINT('Ctrl Pts',(2.6135041541326,0.482896036662513,-1.28848717445863E-16));
#21298=CARTESIAN_POINT('Ctrl Pts',(2.60343298467484,0.516620214186245,-4.06891175216909E-16));
#21299=CARTESIAN_POINT('Ctrl Pts',(2.592718513,0.550160020505481,-5.82867087928207E-16));
#21300=CARTESIAN_POINT('Ctrl Pts',(2.58640686113371,0.569917558494655,-6.86530500515623E-16));
#21301=CARTESIAN_POINT('Ctrl Pts',(2.57987196088238,0.589611101451674,-5.51406606223906E-16));
#21302=CARTESIAN_POINT('Ctrl Pts',(2.57311372784884,0.609235684372638,-7.21644966006352E-16));
#21303=CARTESIAN_POINT('Ctrl Pts',(2.56765136113167,0.625097325729763,-8.59240746715142E-16));
#21304=CARTESIAN_POINT('Ctrl Pts',(2.56204545311482,0.640906940190805,1.0191622183722E-15));
#21305=CARTESIAN_POINT('Ctrl Pts',(2.55629874325467,0.656655644997032,1.08246744900953E-15));
#21306=CARTESIAN_POINT('Ctrl Pts',(2.52550685343402,0.741039996219253,1.42166809325501E-15));
#21307=CARTESIAN_POINT('Ctrl Pts',(2.49065541114871,0.823737254187918,2.9255481979655E-15));
#21308=CARTESIAN_POINT('Ctrl Pts',(2.45179432548469,0.904376871334311,3.03229663600746E-15));
#21309=CARTESIAN_POINT('Ctrl Pts',(2.42326928916242,0.96356842424157,3.11065273492912E-15));
#21310=CARTESIAN_POINT('Ctrl Pts',(2.39258299461189,1.0216508685957,2.15271533017043E-15));
#21311=CARTESIAN_POINT('Ctrl Pts',(2.35974245541383,1.07846525592557,2.35922392732846E-15));
#21312=CARTESIAN_POINT('Ctrl Pts',(2.3470744452395,1.1003810117054,2.43888318609111E-15));
#21313=CARTESIAN_POINT('Ctrl Pts',(2.33408578165144,1.12210795602091,1.70584578534577E-15));
#21314=CARTESIAN_POINT('Ctrl Pts',(2.32077647825335,1.14363645354687,1.81799020282369E-15));
#21315=CARTESIAN_POINT('Ctrl Pts',(2.30811732205646,1.16411330381573,1.92465646889336E-15));
#21316=CARTESIAN_POINT('Ctrl Pts',(2.29516525813278,1.18441464884107,-2.41812693860714E-17));
#21317=CARTESIAN_POINT('Ctrl Pts',(2.28193698658913,1.20450712017389,0.));
#21318=CARTESIAN_POINT('Ctrl Pts',(2.23464326966583,1.27634172444316,8.6452875223902E-17));
#21319=CARTESIAN_POINT('Ctrl Pts',(2.18378846776941,1.34556635950281,1.71218066021624E-15));
#21320=CARTESIAN_POINT('Ctrl Pts',(2.1293995805356,1.4118263229903,7.73686670285656E-16));
#21321=CARTESIAN_POINT('Ctrl Pts',(2.09060596956493,1.45908713999166,1.04293112238207E-16));
#21322=CARTESIAN_POINT('Ctrl Pts',(2.05001367990221,1.50483902366414,-3.15793211228134E-16));
#21323=CARTESIAN_POINT('Ctrl Pts',(2.00762309288065,1.54893995061572,-2.67147415300428E-16));
#21324=CARTESIAN_POINT('Ctrl Pts',(1.9782489136182,1.57949929468088,-2.39592455248551E-16));
#21325=CARTESIAN_POINT('Ctrl Pts',(1.94801102665337,1.60926561951879,-8.19373708274163E-16));
#21326=CARTESIAN_POINT('Ctrl Pts',(1.91694983752522,1.63822102714876,-8.32667268468867E-16));
#21327=CARTESIAN_POINT('Ctrl Pts',(1.91346599666506,1.63598720337495,5.));
#21328=CARTESIAN_POINT('Ctrl Pts',(1.97511426248036,1.57805297138613,5.));
#21329=CARTESIAN_POINT('Ctrl Pts',(2.0333992327661,1.51697077668011,5.));
#21330=CARTESIAN_POINT('Ctrl Pts',(2.08832045660242,1.45312471107507,5.));
#21331=CARTESIAN_POINT('Ctrl Pts',(2.14469107178614,1.38759372425762,5.));
#21332=CARTESIAN_POINT('Ctrl Pts',(2.19751849836391,1.31915063045882,5.));
#21333=CARTESIAN_POINT('Ctrl Pts',(2.2467768545975,1.24816218982756,5.));
#21334=CARTESIAN_POINT('Ctrl Pts',(2.29674569779122,1.17614983436752,5.));
#21335=CARTESIAN_POINT('Ctrl Pts',(2.34304221736815,1.10151755915666,5.));
#21336=CARTESIAN_POINT('Ctrl Pts',(2.38560686750513,1.02460707565943,5.));
#21337=CARTESIAN_POINT('Ctrl Pts',(2.40516281592033,0.989271240805406,5.));
#21338=CARTESIAN_POINT('Ctrl Pts',(2.42393052938809,0.953453999419588,5.));
#21339=CARTESIAN_POINT('Ctrl Pts',(2.44190157522008,0.917186211225675,5.));
#21340=CARTESIAN_POINT('Ctrl Pts',(2.45212589418763,0.896552273823891,5.));
#21341=CARTESIAN_POINT('Ctrl Pts',(2.46209231213777,0.875772477886718,5.));
#21342=CARTESIAN_POINT('Ctrl Pts',(2.47179901297218,0.854852339979442,5.));
#21343=CARTESIAN_POINT('Ctrl Pts',(2.47986584870041,0.837466482643475,5.));
#21344=CARTESIAN_POINT('Ctrl Pts',(2.48775529546885,0.819978882487774,5.));
#21345=CARTESIAN_POINT('Ctrl Pts',(2.49545397654565,0.802421362463391,5.));
#21346=CARTESIAN_POINT('Ctrl Pts',(2.53207516621785,0.718903515111055,5.));
#21347=CARTESIAN_POINT('Ctrl Pts',(2.56443375074574,0.633702408588491,5.));
#21348=CARTESIAN_POINT('Ctrl Pts',(2.59250161927242,0.547215516795963,5.));
#21349=CARTESIAN_POINT('Ctrl Pts',(2.62102734916793,0.459317794443813,5.));
#21350=CARTESIAN_POINT('Ctrl Pts',(2.64512173324747,0.370091241926015,5.));
#21351=CARTESIAN_POINT('Ctrl Pts',(2.6647162612932,0.279916019321374,5.));
#21352=CARTESIAN_POINT('Ctrl Pts',(2.68327377745922,0.194513189135613,5.));
#21353=CARTESIAN_POINT('Ctrl Pts',(2.69779512543597,0.108258519972062,5.));
#21354=CARTESIAN_POINT('Ctrl Pts',(2.70818462605886,0.0214547457753918,
5.));
#21355=CARTESIAN_POINT('Ctrl Pts',(2.71280315092634,-0.0171328056643356,
5.));
#21356=CARTESIAN_POINT('Ctrl Pts',(2.71660465425308,-0.0558290637111655,
5.));
#21357=CARTESIAN_POINT('Ctrl Pts',(2.71957815680565,-0.0946081258455055,
5.));
#21358=CARTESIAN_POINT('Ctrl Pts',(2.72114193269849,-0.115002176780577,
5.));
#21359=CARTESIAN_POINT('Ctrl Pts',(2.72247667707736,-0.135419134083706,
5.));
#21360=CARTESIAN_POINT('Ctrl Pts',(2.72358060529281,-0.155855252406095,
5.));
#21361=CARTESIAN_POINT('Ctrl Pts',(2.72440760299952,-0.171164783180025,
5.));
#21362=CARTESIAN_POINT('Ctrl Pts',(2.72510503301269,-0.186486473786052,
5.));
#21363=CARTESIAN_POINT('Ctrl Pts',(2.72567165779787,-0.201800403224458,
5.));
#21364=CARTESIAN_POINT('Ctrl Pts',(2.72919576912562,-0.297045075921046,
5.));
#21365=CARTESIAN_POINT('Ctrl Pts',(2.72767362176579,-0.39214594976183,5.));
#21366=CARTESIAN_POINT('Ctrl Pts',(2.72104232884131,-0.48670474660219,5.));
#21367=CARTESIAN_POINT('Ctrl Pts',(2.71460574319996,-0.578487118597797,
5.));
#21368=CARTESIAN_POINT('Ctrl Pts',(2.70335577583384,-0.669759723511558,
5.));
#21369=CARTESIAN_POINT('Ctrl Pts',(2.68719094334706,-0.76017485193479,5.));
#21370=CARTESIAN_POINT('Ctrl Pts',(2.67098570391041,-0.850815989477801,
5.));
#21371=CARTESIAN_POINT('Ctrl Pts',(2.64984154989292,-0.940596245438192,
5.));
#21372=CARTESIAN_POINT('Ctrl Pts',(2.62403295621111,-1.02927270988445,5.));
#21373=CARTESIAN_POINT('Ctrl Pts',(2.60893641023223,-1.08114335185981,5.));
#21374=CARTESIAN_POINT('Ctrl Pts',(2.59224287435959,-1.13263631317645,5.));
#21375=CARTESIAN_POINT('Ctrl Pts',(2.57399925344803,-1.18370190437231,5.));
#21376=CARTESIAN_POINT('Ctrl Pts',(2.56913720383633,-1.19731123330153,5.));
#21377=CARTESIAN_POINT('Ctrl Pts',(2.5641650271584,-1.21089020050661,5.));
#21378=CARTESIAN_POINT('Ctrl Pts',(2.55908354497344,-1.22443784743359,5.));
#21379=CARTESIAN_POINT('Ctrl Pts',(2.55395835978812,-1.23810201013234,5.));
#21380=CARTESIAN_POINT('Ctrl Pts',(2.5487251194683,-1.25172589600239,5.));
#21381=CARTESIAN_POINT('Ctrl Pts',(2.54338628977321,-1.26530561093663,5.));
#21382=CARTESIAN_POINT('Ctrl Pts',(2.507474434899,-1.35665011521995,5.));
#21383=CARTESIAN_POINT('Ctrl Pts',(2.46677381849346,-1.44603954020521,5.));
#21384=CARTESIAN_POINT('Ctrl Pts',(2.42165814194307,-1.53319842974304,5.));
#21385=CARTESIAN_POINT('Ctrl Pts',(2.37698904164233,-1.61949457947533,5.));
#21386=CARTESIAN_POINT('Ctrl Pts',(2.32799127252537,-1.70360490076703,5.));
#21387=CARTESIAN_POINT('Ctrl Pts',(2.27497065048649,-1.78525830139829,5.));
#21388=CARTESIAN_POINT('Ctrl Pts',(2.22143189817264,-1.86770963870577,5.));
#21389=CARTESIAN_POINT('Ctrl Pts',(2.16379086711139,-1.94765663398949,5.));
#21390=CARTESIAN_POINT('Ctrl Pts',(2.10231135200038,-2.02480429723545,5.));
#21391=CARTESIAN_POINT('Ctrl Pts',(2.07897018428145,-2.05409399712484,5.));
#21392=CARTESIAN_POINT('Ctrl Pts',(2.05507524958568,-2.08297997370897,5.));
#21393=CARTESIAN_POINT('Ctrl Pts',(2.03063928040512,-2.11144510112202,5.));
#21394=CARTESIAN_POINT('Ctrl Pts',(2.01356866368511,-2.13133042985048,5.));
#21395=CARTESIAN_POINT('Ctrl Pts',(1.99623399133744,-2.1510103628177,5.));
#21396=CARTESIAN_POINT('Ctrl Pts',(1.97863935752325,-2.17047886391133,5.));
#21397=CARTESIAN_POINT('Ctrl Pts',(1.96848269337448,-2.18171723517703,5.));
#21398=CARTESIAN_POINT('Ctrl Pts',(1.95824201635888,-2.19288219327417,5.));
#21399=CARTESIAN_POINT('Ctrl Pts',(1.94792378478368,-2.20396685638102,5.));
#21400=CARTESIAN_POINT('Ctrl Pts',(1.87693652902952,-2.28022699933091,5.));
#21401=CARTESIAN_POINT('Ctrl Pts',(1.80220735563424,-2.35277244990143,5.));
#21402=CARTESIAN_POINT('Ctrl Pts',(1.7240709087608,-2.42127737465979,5.));
#21403=CARTESIAN_POINT('Ctrl Pts',(1.66546857360572,-2.47265606822857,5.));
#21404=CARTESIAN_POINT('Ctrl Pts',(1.60494837513541,-2.52176172516572,5.));
#21405=CARTESIAN_POINT('Ctrl Pts',(1.5426329601745,-2.56844590489654,5.));
#21406=CARTESIAN_POINT('Ctrl Pts',(1.50966649198766,-2.5931430448721,5.));
#21407=CARTESIAN_POINT('Ctrl Pts',(1.47619735041169,-2.61716230488521,5.));
#21408=CARTESIAN_POINT('Ctrl Pts',(1.44224214591351,-2.64048025951079,5.));
#21409=CARTESIAN_POINT('Ctrl Pts',(1.42523499995595,-2.65215952528491,5.));
#21410=CARTESIAN_POINT('Ctrl Pts',(1.40811304383442,-2.66365787868399,5.));
#21411=CARTESIAN_POINT('Ctrl Pts',(1.39088369966999,-2.6749695061669,5.));
#21412=CARTESIAN_POINT('Ctrl Pts',(1.30563891492228,-2.73093549307415,5.));
#21413=CARTESIAN_POINT('Ctrl Pts',(1.2177306352799,-2.78235921066159,5.));
#21414=CARTESIAN_POINT('Ctrl Pts',(1.12744207813993,-2.82892525415745,5.));
#21415=CARTESIAN_POINT('Ctrl Pts',(1.06580281768531,-2.86071551168622,5.));
#21416=CARTESIAN_POINT('Ctrl Pts',(1.00305327491768,-2.89024121467184,5.));
#21417=CARTESIAN_POINT('Ctrl Pts',(0.939273877630842,-2.91739189131414,
5.));
#21418=CARTESIAN_POINT('Ctrl Pts',(0.891985416295931,-2.93752243153926,
5.));
#21419=CARTESIAN_POINT('Ctrl Pts',(0.84413064869809,-2.95634718738556,5.));
#21420=CARTESIAN_POINT('Ctrl Pts',(0.795759619474682,-2.97387964574988,
5.));
#21421=CARTESIAN_POINT('Ctrl Pts',(-2.51589013302272,-0.00197902614912163,
3.38741669750803));
#21422=CARTESIAN_POINT('Ctrl Pts',(-2.51781607531079,-0.253199548871946,
3.40327713660639));
#21423=CARTESIAN_POINT('Ctrl Pts',(-2.48311008876547,-0.503899930938732,
3.41913757570475));
#21424=CARTESIAN_POINT('Ctrl Pts',(-2.40953623658284,-0.742620570455294,
3.43499801480311));
#21425=CARTESIAN_POINT('Ctrl Pts',(-2.16754372508865,-1.52779907325704,
3.48716474764301));
#21426=CARTESIAN_POINT('Ctrl Pts',(-1.50506907192147,-2.18337777113987,
3.5393314804829));
#21427=CARTESIAN_POINT('Ctrl Pts',(-0.717403027393835,-2.41715816749602,
3.5914982133228));
#21428=CARTESIAN_POINT('Ctrl Pts',(0.0702630171338087,-2.65093856385218,
3.64366494616269));
#21429=CARTESIAN_POINT('Ctrl Pts',(0.983120453021916,-2.46292065868166,
3.69583167900259));
#21430=CARTESIAN_POINT('Ctrl Pts',(1.61427619242997,-1.93687739549307,3.74799841184249));
#21431=CARTESIAN_POINT('Ctrl Pts',(2.24543193183803,-1.41083413230447,3.80016514468238));
#21432=CARTESIAN_POINT('Ctrl Pts',(2.59488597476604,-0.546765511097805,
3.85233187752228));
#21433=CARTESIAN_POINT('Ctrl Pts',(2.50687015370919,0.270115932309816,3.90449861036218));
#21434=CARTESIAN_POINT('Ctrl Pts',(2.41885433265234,1.08699737571744,3.95666534320207));
#21435=CARTESIAN_POINT('Ctrl Pts',(1.89336864761064,1.85669164132601,4.00883207604197));
#21436=CARTESIAN_POINT('Ctrl Pts',(1.16464828769536,2.23624130185117,4.06099880888186));
#21437=CARTESIAN_POINT('Ctrl Pts',(0.435927927780085,2.61579096237633,4.11316554172176));
#21438=CARTESIAN_POINT('Ctrl Pts',(-0.496027107008767,2.60519601781808,
4.16533227456166));
#21439=CARTESIAN_POINT('Ctrl Pts',(-1.21582191903011,2.20894048902741,4.21749900740156));
#21440=CARTESIAN_POINT('Ctrl Pts',(-1.93561673105145,1.81268496023674,4.26966574024145));
#21441=CARTESIAN_POINT('Ctrl Pts',(-2.44325132030528,1.03076884721365,4.32183247308135));
#21442=CARTESIAN_POINT('Ctrl Pts',(-2.51242976891092,0.212180128913875,
4.37399920592124));
#21443=CARTESIAN_POINT('Ctrl Pts',(-2.51836075980379,0.141998702022978,
4.37847170311684));
#21444=CARTESIAN_POINT('Ctrl Pts',(-2.52106890854963,0.0715477156323498,
4.38294420031243));
#21445=CARTESIAN_POINT('Ctrl Pts',(-2.52065797473119,0.00106685237120291,
4.38741669750802));
#21446=CARTESIAN_POINT('Ctrl Pts',(-0.793799282532885,-2.96922295374569,
5.));
#21447=CARTESIAN_POINT('Ctrl Pts',(-1.76703113798775,-2.70903678361534,
4.9478332671601));
#21448=CARTESIAN_POINT('Ctrl Pts',(-3.42227762319113,-1.16284338723151,
4.84349980148031));
#21449=CARTESIAN_POINT('Ctrl Pts',(-2.86382437134345,2.21031103269041,4.68699960296062));
#21450=CARTESIAN_POINT('Ctrl Pts',(0.252054090990421,3.60562829022214,4.53049940444094));
#21451=CARTESIAN_POINT('Ctrl Pts',(3.14100203598835,1.79029184281612,4.37399920592124));
#21452=CARTESIAN_POINT('Ctrl Pts',(3.23098071080095,-1.62294021205589,4.21749900740156));
#21453=CARTESIAN_POINT('Ctrl Pts',(0.440018754334274,-3.58837598279832,
4.06099880888186));
#21454=CARTESIAN_POINT('Ctrl Pts',(-2.74289544065113,-2.35537722830823,
3.90449861036218));
#21455=CARTESIAN_POINT('Ctrl Pts',(-3.48074999950888,0.977649265989379,
3.74799841184248));
#21456=CARTESIAN_POINT('Ctrl Pts',(-1.11551737463701,3.43898632522653,3.5914982133228));
#21457=CARTESIAN_POINT('Ctrl Pts',(2.24412684766706,2.83462531411003,3.43499801480311));
#21458=CARTESIAN_POINT('Ctrl Pts',(3.60321095550619,-0.296771509319279,
3.27849781628342));
#21459=CARTESIAN_POINT('Ctrl Pts',(1.75011009124083,-3.16358418358746,3.12199761776373));
#21460=CARTESIAN_POINT('Ctrl Pts',(-1.66316409145381,-3.2101505430571,2.96549741924404));
#21461=CARTESIAN_POINT('Ctrl Pts',(-3.59377214139091,-0.394942236718185,
2.80899722072435));
#21462=CARTESIAN_POINT('Ctrl Pts',(-2.3206200405613,2.77234451758071,2.65249702220466));
#21463=CARTESIAN_POINT('Ctrl Pts',(1.02130620401276,3.46815644429995,2.49599682368497));
#21464=CARTESIAN_POINT('Ctrl Pts',(3.45276382958855,1.07219267437738,2.33949662516528));
#21465=CARTESIAN_POINT('Ctrl Pts',(2.8061681927767,-2.27960425476498,2.18299642664559));
#21466=CARTESIAN_POINT('Ctrl Pts',(-0.34205648942751,-3.59919002761108,
2.02649622812591));
#21467=CARTESIAN_POINT('Ctrl Pts',(-3.18534629574052,-1.71018903949051,
1.86999602960622));
#21468=CARTESIAN_POINT('Ctrl Pts',(-3.18897927637007,1.7034061403768,1.71349583108653));
#21469=CARTESIAN_POINT('Ctrl Pts',(-0.349716256635896,3.59845088308181,
1.55699563256684));
#21470=CARTESIAN_POINT('Ctrl Pts',(2.8013094644448,2.28557822072128,1.40049543404715));
#21471=CARTESIAN_POINT('Ctrl Pts',(3.45503873870173,-1.0648536490447,1.24399523552746));
#21472=CARTESIAN_POINT('Ctrl Pts',(1.02868455419652,-3.46595066989846,1.08749503700777));
#21473=CARTESIAN_POINT('Ctrl Pts',(-2.31471172988138,-2.77732393751975,
0.930994838488083));
#21474=CARTESIAN_POINT('Ctrl Pts',(-3.5946088997546,0.387381135037168,0.774494639968393));
#21475=CARTESIAN_POINT('Ctrl Pts',(-1.66998478533906,3.20643252148329,0.617994441448703));
#21476=CARTESIAN_POINT('Ctrl Pts',(1.74335679702331,3.1676297706248,0.461494242929015));
#21477=CARTESIAN_POINT('Ctrl Pts',(3.60260150316633,0.3038109312067,0.304994044409326));
#21478=CARTESIAN_POINT('Ctrl Pts',(2.25009578791265,-2.82863139649778,0.148493845889636));
#21479=CARTESIAN_POINT('Ctrl Pts',(-1.10807133015233,-3.44371061769541,
-0.00800635263005217));
#21480=CARTESIAN_POINT('Ctrl Pts',(-3.47898841388462,-0.980218592702346,
-0.164506551149742));
#21481=CARTESIAN_POINT('Ctrl Pts',(-2.99072467884965,1.23160270904172,-0.268840016829535));
#21482=CARTESIAN_POINT('Ctrl Pts',(-2.33606265769614,1.99730155693066,-0.321006749669431));
#21483=CARTESIAN_POINT('Ctrl Pts',(-0.745932854346964,-2.79017756984215,
5.10700224988981));
#21484=CARTESIAN_POINT('Ctrl Pts',(-1.66047842254703,-2.54568073441083,
5.05483551704991));
#21485=CARTESIAN_POINT('Ctrl Pts',(-3.21591285354802,-1.09272344543869,
4.95050205137012));
#21486=CARTESIAN_POINT('Ctrl Pts',(-2.69113456596771,2.07702835450855,4.79400185285043));
#21487=CARTESIAN_POINT('Ctrl Pts',(0.236855124059054,3.38820739879938,4.63750165433075));
#21488=CARTESIAN_POINT('Ctrl Pts',(2.95159830169959,1.68233649716179,4.48100145581105));
#21489=CARTESIAN_POINT('Ctrl Pts',(3.03615122485059,-1.52507623961371,4.32450125729137));
#21490=CARTESIAN_POINT('Ctrl Pts',(0.413485439719026,-3.37199541271688,
4.16800105877167));
#21491=CARTESIAN_POINT('Ctrl Pts',(-2.57749770028975,-2.21334699795853,
4.01150086025199));
#21492=CARTESIAN_POINT('Ctrl Pts',(-3.2708593211588,0.918696607034865,3.85500066173229));
#21493=CARTESIAN_POINT('Ctrl Pts',(-1.04825121116451,3.231614013874,3.69850046321261));
#21494=CARTESIAN_POINT('Ctrl Pts',(2.10880506172238,2.66369622407748,3.54200026469292));
#21495=CARTESIAN_POINT('Ctrl Pts',(3.38593583037616,-0.278876063391019,
3.38550006617323));
#21496=CARTESIAN_POINT('Ctrl Pts',(1.64457772198429,-2.97281873636934,3.22899986765354));
#21497=CARTESIAN_POINT('Ctrl Pts',(-1.56287460228854,-3.01657712491928,
3.07249966913385));
#21498=CARTESIAN_POINT('Ctrl Pts',(-3.37706618069319,-0.371127054936794,
2.91599947061416));
#21499=CARTESIAN_POINT('Ctrl Pts',(-2.18068568314553,2.60517098558408,2.75949927209447));
#21500=CARTESIAN_POINT('Ctrl Pts',(0.95972101346657,3.25902516258738,2.60299907357479));
#21501=CARTESIAN_POINT('Ctrl Pts',(3.24456072897023,1.00753900842068,2.44649887505509));
#21502=CARTESIAN_POINT('Ctrl Pts',(2.63695507904276,-2.14214316635878,2.28999867653541));
#21503=CARTESIAN_POINT('Ctrl Pts',(-0.321430340290076,-3.38215736611206,
2.13349847801571));
#21504=CARTESIAN_POINT('Ctrl Pts',(-2.99326858407285,-1.60706392632346,
1.97699827949603));
#21505=CARTESIAN_POINT('Ctrl Pts',(-2.9966824944535,1.60069003885849,1.82049808097634));
#21506=CARTESIAN_POINT('Ctrl Pts',(-0.32862822033748,3.38146279230653,1.66399788245665));
#21507=CARTESIAN_POINT('Ctrl Pts',(2.63238933405802,2.1477568996735,1.50749768393696));
#21508=CARTESIAN_POINT('Ctrl Pts',(3.246698460114,-1.00064252937995,1.35099748541727));
#21509=CARTESIAN_POINT('Ctrl Pts',(0.96665444605344,-3.25695239730331,1.19449728689758));
#21510=CARTESIAN_POINT('Ctrl Pts',(-2.17513364606662,-2.60985014442166,
1.03799708837789));
#21511=CARTESIAN_POINT('Ctrl Pts',(-3.37785248217816,0.364021890844269,
0.881496889858204));
#21512=CARTESIAN_POINT('Ctrl Pts',(-1.56928400548455,3.01308330159882,0.724996691338513));
#21513=CARTESIAN_POINT('Ctrl Pts',(1.63823165422791,2.9766203728191,0.568496492818826));
#21514=CARTESIAN_POINT('Ctrl Pts',(3.38536312826686,0.285491005199331,0.411996294299136));
#21515=CARTESIAN_POINT('Ctrl Pts',(2.11441407237884,-2.65806374219999,0.255496095779446));
#21516=CARTESIAN_POINT('Ctrl Pts',(-1.04125416627134,-3.2360534295344,0.0989958972597585));
#21517=CARTESIAN_POINT('Ctrl Pts',(-3.26920395988323,-0.921111002274222,
-0.0575043012599318));
#21518=CARTESIAN_POINT('Ctrl Pts',(-2.81038273194434,1.15733655143344,-0.161837766939724));
#21519=CARTESIAN_POINT('Ctrl Pts',(-2.19519710401911,1.87686343907876,-0.214004499779621));
#21520=CARTESIAN_POINT('Ctrl Pts',(-0.698066426161043,-2.61113218593861,
5.21400449977962));
#21521=CARTESIAN_POINT('Ctrl Pts',(-1.55392570710631,-2.38232468520633,
5.16183776693972));
#21522=CARTESIAN_POINT('Ctrl Pts',(-3.00954808390491,-1.02260350364586,
5.05750430125993));
#21523=CARTESIAN_POINT('Ctrl Pts',(-2.51844476059198,1.94374567632669,4.90100410274025));
#21524=CARTESIAN_POINT('Ctrl Pts',(0.221656157127689,3.17078650737663,4.74450390422055));
#21525=CARTESIAN_POINT('Ctrl Pts',(2.76219456741083,1.57438115150745,4.58800370570087));
#21526=CARTESIAN_POINT('Ctrl Pts',(2.84132173890023,-1.42721226717154,4.43150350718117));
#21527=CARTESIAN_POINT('Ctrl Pts',(0.386952125103784,-3.15561484263544,
4.27500330866149));
#21528=CARTESIAN_POINT('Ctrl Pts',(-2.41209995992838,-2.07131676760884,
4.11850311014179));
#21529=CARTESIAN_POINT('Ctrl Pts',(-3.06096864280872,0.859743948080353,
3.96200291162211));
#21530=CARTESIAN_POINT('Ctrl Pts',(-0.98098504769201,3.02424170252148,3.80550271310242));
#21531=CARTESIAN_POINT('Ctrl Pts',(1.9734832757777,2.49276713404493,3.64900251458273));
#21532=CARTESIAN_POINT('Ctrl Pts',(3.16866070524613,-0.260980617462761,
3.49250231606304));
#21533=CARTESIAN_POINT('Ctrl Pts',(1.53904535272775,-2.78205328915123,3.33600211754335));
#21534=CARTESIAN_POINT('Ctrl Pts',(-1.46258511312328,-2.82300370678147,
3.17950191902366));
#21535=CARTESIAN_POINT('Ctrl Pts',(-3.16036021999547,-0.347311873155402,
3.02300172050397));
#21536=CARTESIAN_POINT('Ctrl Pts',(-2.04075132572976,2.43799745358745,2.86650152198428));
#21537=CARTESIAN_POINT('Ctrl Pts',(0.898135822920388,3.04989388087481,2.7100013234646));
#21538=CARTESIAN_POINT('Ctrl Pts',(3.03635762835191,0.942885342463967,2.5535011249449));
#21539=CARTESIAN_POINT('Ctrl Pts',(2.46774196530881,-2.00468207795258,2.39700092642522));
#21540=CARTESIAN_POINT('Ctrl Pts',(-0.300804191152645,-3.16512470461303,
2.24050072790553));
#21541=CARTESIAN_POINT('Ctrl Pts',(-2.80119087240519,-1.50393881315642,
2.08400052938584));
#21542=CARTESIAN_POINT('Ctrl Pts',(-2.80438571253693,1.49797393734019,1.92750033086615));
#21543=CARTESIAN_POINT('Ctrl Pts',(-0.307540184039062,3.16447470153125,
1.77100013234646));
#21544=CARTESIAN_POINT('Ctrl Pts',(2.46346920367124,2.00993557862573,1.61449993382677));
#21545=CARTESIAN_POINT('Ctrl Pts',(3.03835818152627,-0.936431409715195,
1.45799973530708));
#21546=CARTESIAN_POINT('Ctrl Pts',(0.904624337910361,-3.04795412470817,
1.30149953678739));
#21547=CARTESIAN_POINT('Ctrl Pts',(-2.03555556225185,-2.44237635132356,
1.1449993382677));
#21548=CARTESIAN_POINT('Ctrl Pts',(-3.16109606460172,0.340662646651362,
0.988499139748014));
#21549=CARTESIAN_POINT('Ctrl Pts',(-1.46858322563004,2.81973408171437,0.831998941228325));
#21550=CARTESIAN_POINT('Ctrl Pts',(1.53310651143252,2.78561097501341,0.675498742708636));
#21551=CARTESIAN_POINT('Ctrl Pts',(3.1681247533674,0.267171079191969,0.518998544188947));
#21552=CARTESIAN_POINT('Ctrl Pts',(1.97873235684504,-2.4874960879022,0.362498345669256));
#21553=CARTESIAN_POINT('Ctrl Pts',(-0.974437002390344,-3.02839624137338,
0.205998147149569));
#21554=CARTESIAN_POINT('Ctrl Pts',(-3.05941950588183,-0.862003411846101,
0.0494979486298786));
#21555=CARTESIAN_POINT('Ctrl Pts',(-2.63004078503903,1.08307039382515,-0.0548355170499138));
#21556=CARTESIAN_POINT('Ctrl Pts',(-2.05433155034208,1.75642532122686,-0.10700224988981));
#21557=CARTESIAN_POINT('Ctrl Pts',(-0.650199997975122,-2.43208680203507,
5.32100674966943));
#21558=CARTESIAN_POINT('Ctrl Pts',(-1.44737299166558,-2.21896863600183,
5.26884001682953));
#21559=CARTESIAN_POINT('Ctrl Pts',(-2.80318331426181,-0.952483561853041,
5.16450655114974));
#21560=CARTESIAN_POINT('Ctrl Pts',(-2.34575495521625,1.81046299814482,5.00800635263005));
#21561=CARTESIAN_POINT('Ctrl Pts',(0.206457190196319,2.95336561595388,4.85150615411036));
#21562=CARTESIAN_POINT('Ctrl Pts',(2.57279083312207,1.46642580585312,4.69500595559068));
#21563=CARTESIAN_POINT('Ctrl Pts',(2.64649225294986,-1.32934829472936,4.53850575707098));
#21564=CARTESIAN_POINT('Ctrl Pts',(0.360418810488541,-2.93923427255401,
4.3820055585513));
#21565=CARTESIAN_POINT('Ctrl Pts',(-2.24670221956701,-1.92928653725914,
4.22550536003161));
#21566=CARTESIAN_POINT('Ctrl Pts',(-2.85107796445863,0.800791289125838,
4.06900516151192));
#21567=CARTESIAN_POINT('Ctrl Pts',(-0.913718884219513,2.81686939116895,
3.91250496299223));
#21568=CARTESIAN_POINT('Ctrl Pts',(1.83816148983303,2.32183804401237,3.75600476447254));
#21569=CARTESIAN_POINT('Ctrl Pts',(2.9513855801161,-0.243085171534501,3.59950456595285));
#21570=CARTESIAN_POINT('Ctrl Pts',(1.43351298347121,-2.59128784193311,3.44300436743316));
#21571=CARTESIAN_POINT('Ctrl Pts',(-1.36229562395802,-2.62943028864365,
3.28650416891347));
#21572=CARTESIAN_POINT('Ctrl Pts',(-2.94365425929774,-0.323496691374012,
3.13000397039378));
#21573=CARTESIAN_POINT('Ctrl Pts',(-1.90081696831399,2.27082392159083,2.97350377187409));
#21574=CARTESIAN_POINT('Ctrl Pts',(0.836550632374203,2.84076259916223,2.81700357335441));
#21575=CARTESIAN_POINT('Ctrl Pts',(2.82815452773359,0.878231676507261,2.66050337483472));
#21576=CARTESIAN_POINT('Ctrl Pts',(2.29852885157487,-1.86722098954639,2.50400317631502));
#21577=CARTESIAN_POINT('Ctrl Pts',(-0.280178042015212,-2.948092043114,2.34750297779534));
#21578=CARTESIAN_POINT('Ctrl Pts',(-2.60911316073752,-1.40081369998938,
2.19100277927565));
#21579=CARTESIAN_POINT('Ctrl Pts',(-2.61208893062035,1.39525783582189,2.03450258075596));
#21580=CARTESIAN_POINT('Ctrl Pts',(-0.286452147740644,2.94748661075597,
1.87800238223627));
#21581=CARTESIAN_POINT('Ctrl Pts',(2.29454907328446,1.87211425757795,1.72150218371658));
#21582=CARTESIAN_POINT('Ctrl Pts',(2.83001790293854,-0.872220290050442,
1.56500198519689));
#21583=CARTESIAN_POINT('Ctrl Pts',(0.842594229767281,-2.83895585211302,
1.4085017866772));
#21584=CARTESIAN_POINT('Ctrl Pts',(-1.89597747843709,-2.27490255822547,
1.25200158815751));
#21585=CARTESIAN_POINT('Ctrl Pts',(-2.94433964702528,0.317303402458459,
1.09550138963782));
#21586=CARTESIAN_POINT('Ctrl Pts',(-1.36788244577553,2.6263848618299,0.939001191118136));
#21587=CARTESIAN_POINT('Ctrl Pts',(1.42798136863712,2.59460157720772,0.782500992598445));
#21588=CARTESIAN_POINT('Ctrl Pts',(2.95088637846794,0.248851153184599,0.626000794078758));
#21589=CARTESIAN_POINT('Ctrl Pts',(1.84305064131124,-2.31692843360441,0.469500595559067));
#21590=CARTESIAN_POINT('Ctrl Pts',(-0.907619838509351,-2.82073905321236,
0.31300039703938));
#21591=CARTESIAN_POINT('Ctrl Pts',(-2.84963505188044,-0.802895821417979,
0.156500198519689));
#21592=CARTESIAN_POINT('Ctrl Pts',(-2.44969883813372,1.00880423621686,0.0521667328398966));
#21593=CARTESIAN_POINT('Ctrl Pts',(-1.91346599666505,1.63598720337496,0.));
#21594=CARTESIAN_POINT('Ctrl Pts',(-1.91346599666505,1.63598720337496,0.));
#21595=CARTESIAN_POINT('Ctrl Pts',(-1.97511445450674,1.57805279092849,-2.16023702375061E-17));
#21596=CARTESIAN_POINT('Ctrl Pts',(-2.03339962644492,1.51697042789119,-3.49443898869507E-17));
#21597=CARTESIAN_POINT('Ctrl Pts',(-2.08832105501608,1.45312420295415,-1.11022302462516E-16));
#21598=CARTESIAN_POINT('Ctrl Pts',(-2.1446918579957,1.38759307857242,-1.89107908253736E-16));
#21599=CARTESIAN_POINT('Ctrl Pts',(-2.19751947843796,1.31914985899599,-1.96056269520747E-15));
#21600=CARTESIAN_POINT('Ctrl Pts',(-2.2467780277058,1.24816130047737,-2.16493489801906E-15));
#21601=CARTESIAN_POINT('Ctrl Pts',(-2.29674689545117,1.17614907224947,-2.37225419030257E-15));
#21602=CARTESIAN_POINT('Ctrl Pts',(-2.34304346389473,1.10151695033136,8.04059381600243E-19));
#21603=CARTESIAN_POINT('Ctrl Pts',(-2.38560818063646,1.02460663863002,2.77555756156289E-16));
#21604=CARTESIAN_POINT('Ctrl Pts',(-2.40516403209366,0.989271113192736,
4.04706022549276E-16));
#21605=CARTESIAN_POINT('Ctrl Pts',(-2.42393166263322,0.953454191414296,
1.85001145283656E-16));
#21606=CARTESIAN_POINT('Ctrl Pts',(-2.44190263911885,0.917186731710372,
2.77555756156289E-16));
#21607=CARTESIAN_POINT('Ctrl Pts',(-2.45212691902149,0.896552980413291,
3.30213120022811E-16));
#21608=CARTESIAN_POINT('Ctrl Pts',(-2.46209330228438,0.875773373445736,
1.0101923078241E-15));
#21609=CARTESIAN_POINT('Ctrl Pts',(-2.47179997273461,0.85485342713836,9.99200722162641E-16));
#21610=CARTESIAN_POINT('Ctrl Pts',(-2.47986685205683,0.837467580657393,
9.90065994086157E-16));
#21611=CARTESIAN_POINT('Ctrl Pts',(-2.48775634234785,0.819979991507439,
-1.29538532938285E-15));
#21612=CARTESIAN_POINT('Ctrl Pts',(-2.49545506671926,0.802422482605945,
-1.22124532708767E-15));
#21613=CARTESIAN_POINT('Ctrl Pts',(-2.53207648579799,0.718904634655909,
-8.68574941246235E-16));
#21614=CARTESIAN_POINT('Ctrl Pts',(-2.56443528935485,0.633703528135737,
-2.73580965033665E-16));
#21615=CARTESIAN_POINT('Ctrl Pts',(-2.59250335927894,0.547216632073775,
-2.22044604925031E-16));
#21616=CARTESIAN_POINT('Ctrl Pts',(-2.62102926303655,0.45931900035097,-1.696676067042E-16));
#21617=CARTESIAN_POINT('Ctrl Pts',(-2.64512381235207,0.370092536921413,
8.62583150244892E-16));
#21618=CARTESIAN_POINT('Ctrl Pts',(-2.6647184895653,0.279917395525893,9.71445146547012E-16));
#21619=CARTESIAN_POINT('Ctrl Pts',(-2.68327611608723,0.194514784532604,
1.07454560836236E-15));
#21620=CARTESIAN_POINT('Ctrl Pts',(-2.69779757345701,0.108260330337431,
1.58880599429527E-15));
#21621=CARTESIAN_POINT('Ctrl Pts',(-2.70818717658801,0.0214567600039818,
1.52655665885959E-15));
#21622=CARTESIAN_POINT('Ctrl Pts',(-2.71280574576047,-0.0171306902524466,
1.49888448909292E-15));
#21623=CARTESIAN_POINT('Ctrl Pts',(-2.71660729247955,-0.0558268492504973,
1.27797020542778E-15));
#21624=CARTESIAN_POINT('Ctrl Pts',(-2.71958083700161,-0.0946058150986653,
1.2490009027033E-15));
#21625=CARTESIAN_POINT('Ctrl Pts',(-2.72114459889708,-0.114999345005228,
1.23376619160252E-15));
#21626=CARTESIAN_POINT('Ctrl Pts',(-2.72247933944975,-0.135415780987334,
2.7744501595987E-15));
#21627=CARTESIAN_POINT('Ctrl Pts',(-2.72358327406089,-0.155851378047186,
2.83106871279415E-15));
#21628=CARTESIAN_POINT('Ctrl Pts',(-2.72441031908349,-0.171161305520925,
2.87348616409501E-15));
#21629=CARTESIAN_POINT('Ctrl Pts',(-2.72510778883702,-0.186483394270956,
-3.27116286657501E-16));
#21630=CARTESIAN_POINT('Ctrl Pts',(-2.72567444563692,-0.201797722043239,
-3.05311331771918E-16));
#21631=CARTESIAN_POINT('Ctrl Pts',(-2.72919865876058,-0.297042242048632,
-1.69699603154258E-16));
#21632=CARTESIAN_POINT('Ctrl Pts',(-2.7276765940473,-0.392142984842673,
1.65684655347014E-15));
#21633=CARTESIAN_POINT('Ctrl Pts',(-2.72104535728848,-0.486701680153984,
1.80411241501588E-15));
#21634=CARTESIAN_POINT('Ctrl Pts',(-2.71460882823241,-0.578483924102048,
1.94705422681979E-15));
#21635=CARTESIAN_POINT('Ctrl Pts',(-2.70335889560743,-0.669756429091281,
-1.44907627993903E-16));
#21636=CARTESIAN_POINT('Ctrl Pts',(-2.68719406942169,-0.760171493259568,
-2.4980018054066E-16));
#21637=CARTESIAN_POINT('Ctrl Pts',(-2.67098885106311,-0.850812483822458,
-3.27199259771174E-16));
#21638=CARTESIAN_POINT('Ctrl Pts',(-2.64984469854827,-0.940592630196976,
2.00672834831372E-15));
#21639=CARTESIAN_POINT('Ctrl Pts',(-2.62403609171522,-1.02926901742914,
1.97064586870965E-15));
#21640=CARTESIAN_POINT('Ctrl Pts',(-2.60893951244934,-1.08113970217868,
1.94953965336933E-15));
#21641=CARTESIAN_POINT('Ctrl Pts',(-2.59224593286086,-1.13263271607333,
1.51263892527377E-15));
#21642=CARTESIAN_POINT('Ctrl Pts',(-2.57400225902127,-1.18369836845093,
1.4432899320127E-15));
#21643=CARTESIAN_POINT('Ctrl Pts',(-2.56914004859136,-1.19730812434678,
1.42480739382975E-15));
#21644=CARTESIAN_POINT('Ctrl Pts',(-2.56416770379457,-1.21088751729747,
1.46101747209947E-15));
#21645=CARTESIAN_POINT('Ctrl Pts',(-2.55908604628673,-1.22443558863974,
1.41553435639707E-15));
#21646=CARTESIAN_POINT('Ctrl Pts',(-2.55396092950485,-1.23809952559165,
1.36966226068444E-15));
#21647=CARTESIAN_POINT('Ctrl Pts',(-2.54872776110117,-1.25172318692358,
7.2111001976691E-16));
#21648=CARTESIAN_POINT('Ctrl Pts',(-2.54338900633193,-1.26530267978209,
8.04911692853238E-16));
#21649=CARTESIAN_POINT('Ctrl Pts',(-2.50747702892334,-1.35664728387668,
1.36861688643376E-15));
#21650=CARTESIAN_POINT('Ctrl Pts',(-2.46677626545746,-1.44603683426546,
3.98698161417476E-15));
#21651=CARTESIAN_POINT('Ctrl Pts',(-2.42166042457756,-1.53319586749654,
3.8441472227646E-15));
#21652=CARTESIAN_POINT('Ctrl Pts',(-2.37699119409271,-1.6194920966769,3.70272677649499E-15));
#21653=CARTESIAN_POINT('Ctrl Pts',(-2.32799328414659,-1.70360251853944,
2.71566994649136E-15));
#21654=CARTESIAN_POINT('Ctrl Pts',(-2.27497251664925,-1.78525603476489,
3.10862446895044E-15));
#21655=CARTESIAN_POINT('Ctrl Pts',(-2.22143358365231,-1.86770754085407,
3.50541928807182E-15));
#21656=CARTESIAN_POINT('Ctrl Pts',(-2.16379236200239,-1.94765471708648,
2.12393071997628E-15));
#21657=CARTESIAN_POINT('Ctrl Pts',(-2.10231265300888,-2.02480256688325,
2.24820162486594E-15));
#21658=CARTESIAN_POINT('Ctrl Pts',(-2.07897144804811,-2.05409229196278,
2.29538195003625E-15));
#21659=CARTESIAN_POINT('Ctrl Pts',(-2.05507647736,-2.082978295804,3.52826900319682E-15));
#21660=CARTESIAN_POINT('Ctrl Pts',(-2.03064047373774,-2.11144345226609,
3.52495810318487E-15));
#21661=CARTESIAN_POINT('Ctrl Pts',(-2.01356997979656,-2.13132863023677,
3.52264517593754E-15));
#21662=CARTESIAN_POINT('Ctrl Pts',(-1.99623543552702,-2.15100841685411,
2.17794287054721E-15));
#21663=CARTESIAN_POINT('Ctrl Pts',(-1.97864093508987,-2.17047677606985,
2.02615701994091E-15));
#21664=CARTESIAN_POINT('Ctrl Pts',(-1.96848450504363,-2.18171489159328,
1.93853859740034E-15));
#21665=CARTESIAN_POINT('Ctrl Pts',(-1.95824406587573,-2.19287959838895,
2.78311917693584E-15));
#21666=CARTESIAN_POINT('Ctrl Pts',(-1.94792607632517,-2.20396401413293,
2.80331313717852E-15));
#21667=CARTESIAN_POINT('Ctrl Pts',(-1.87693852294064,-2.28022456377845,
2.94224716340022E-15));
#21668=CARTESIAN_POINT('Ctrl Pts',(-1.80220903731176,-2.35277040780027,
3.04985240962845E-15));
#21669=CARTESIAN_POINT('Ctrl Pts',(-1.72407227353766,-2.42127570338811,
3.40005801291454E-15));
#21670=CARTESIAN_POINT('Ctrl Pts',(-1.66546970070708,-2.472654675079,3.66271221537911E-15));
#21671=CARTESIAN_POINT('Ctrl Pts',(-1.60494926191777,-2.52176059742133,
2.66897608121856E-15));
#21672=CARTESIAN_POINT('Ctrl Pts',(-1.54263360799992,-2.56844502586205,
2.44249065417534E-15));
#21673=CARTESIAN_POINT('Ctrl Pts',(-1.50966712749181,-2.59314221193751,
2.32267441304543E-15));
#21674=CARTESIAN_POINT('Ctrl Pts',(-1.47619797745247,-2.61716151806854,
2.66421769654117E-15));
#21675=CARTESIAN_POINT('Ctrl Pts',(-1.44224276876128,-2.64047951847467,
2.55351295663786E-15));
#21676=CARTESIAN_POINT('Ctrl Pts',(-1.42523529016054,-2.65215903417213,
2.49806318714802E-15));
#21677=CARTESIAN_POINT('Ctrl Pts',(-1.40811299715223,-2.66365763094131,
1.70970381910793E-15));
#21678=CARTESIAN_POINT('Ctrl Pts',(-1.39088331342309,-2.6749694941009,1.85962356624714E-15));
#21679=CARTESIAN_POINT('Ctrl Pts',(-1.30563836789021,-2.73093564960753,
2.60136095853466E-15));
#21680=CARTESIAN_POINT('Ctrl Pts',(-1.21772994683618,-2.78235951649428,
1.84996893450162E-15));
#21681=CARTESIAN_POINT('Ctrl Pts',(-1.12744127475458,-2.82892568298919,
1.45369827286856E-15));
#21682=CARTESIAN_POINT('Ctrl Pts',(-1.06580182053759,-2.86071608395033,
1.18316702302153E-15));
#21683=CARTESIAN_POINT('Ctrl Pts',(-1.00305209219164,-2.89024190964375,
-1.85681498777599E-15));
#21684=CARTESIAN_POINT('Ctrl Pts',(-0.939272520240859,-2.91739268538644,
-2.72698530423554E-15));
#21685=CARTESIAN_POINT('Ctrl Pts',(-0.891984018423086,-2.93752326119295,
-3.3646306259368E-15));
#21686=CARTESIAN_POINT('Ctrl Pts',(-0.844129218472895,-2.95634804455667,
-1.21993627764454E-15));
#21687=CARTESIAN_POINT('Ctrl Pts',(-0.795758164394645,-2.97388052305262,
-1.30451205393456E-15));
#21688=CARTESIAN_POINT('Ctrl Pts',(-2.51644348201823,0.00207613456667446,
4.11258330249198));
#21689=CARTESIAN_POINT('Ctrl Pts',(-2.51833412820368,0.232035413192547,
4.09805725549862));
#21690=CARTESIAN_POINT('Ctrl Pts',(-2.489317966475,0.461526809188866,4.08353120850527));
#21691=CARTESIAN_POINT('Ctrl Pts',(-2.42745549360351,0.681791335068863,
4.06900516151192));
#21692=CARTESIAN_POINT('Ctrl Pts',(-2.20529160437893,1.47281732314021,4.01683842867202));
#21693=CARTESIAN_POINT('Ctrl Pts',(-1.55950524429922,2.14484335715458,3.96467169583213));
#21694=CARTESIAN_POINT('Ctrl Pts',(-0.777965335250612,2.39835114963567,
3.91250496299223));
#21695=CARTESIAN_POINT('Ctrl Pts',(0.00357457379799905,2.65185894211676,
3.86033823015234));
#21696=CARTESIAN_POINT('Ctrl Pts',(0.920868031815514,2.48684849306456,3.80817149731244));
#21697=CARTESIAN_POINT('Ctrl Pts',(1.56505210920478,1.97685606594732,3.75600476447254));
#21698=CARTESIAN_POINT('Ctrl Pts',(2.20923618659405,1.46686363883008,3.70383803163264));
#21699=CARTESIAN_POINT('Ctrl Pts',(2.58031088335508,0.611889233647789,3.65167129879275));
#21700=CARTESIAN_POINT('Ctrl Pts',(2.51286946562811,-0.206965080676461,
3.59950456595285));
#21701=CARTESIAN_POINT('Ctrl Pts',(2.44542804790114,-1.0258193950007,3.54733783311295));
#21702=CARTESIAN_POINT('Ctrl Pts',(1.93947051568617,-1.80855361846691,3.49517110027306));
#21703=CARTESIAN_POINT('Ctrl Pts',(1.22052364834049,-2.20627780465177,3.44300436743316));
#21704=CARTESIAN_POINT('Ctrl Pts',(0.501576780994809,-2.60400199083662,
3.39083763459327));
#21705=CARTESIAN_POINT('Ctrl Pts',(-0.430359421481595,-2.61671613974014,
3.33867090175337));
#21706=CARTESIAN_POINT('Ctrl Pts',(-1.15988729527642,-2.23875094798029,
3.28650416891347));
#21707=CARTESIAN_POINT('Ctrl Pts',(-1.88941516907125,-1.86078575622044,
3.23433743607358));
#21708=CARTESIAN_POINT('Ctrl Pts',(-2.4165347141845,-1.09214122379723,3.18217070323368));
#21709=CARTESIAN_POINT('Ctrl Pts',(-2.50628827157716,-0.275432188758138,
3.13000397039378));
#21710=CARTESIAN_POINT('Ctrl Pts',(-2.51627910181976,-0.18452101416286,
3.12419708109318));
#21711=CARTESIAN_POINT('Ctrl Pts',(-2.52085061170807,-0.0930142812830837,
3.11839019179258));
#21712=CARTESIAN_POINT('Ctrl Pts',(-2.52021651143941,-0.00144364612508765,
3.11258330249198));
#21713=CARTESIAN_POINT('Ctrl Pts',(-0.793799282532885,-2.96922295374569,
5.));
#21714=CARTESIAN_POINT('Ctrl Pts',(-0.886893974343616,-2.93516849963005,
5.));
#21715=CARTESIAN_POINT('Ctrl Pts',(-0.977926652176332,-2.89635378057927,
5.));
#21716=CARTESIAN_POINT('Ctrl Pts',(-1.06668684681747,-2.85310443912188,
5.));
#21717=CARTESIAN_POINT('Ctrl Pts',(-1.15738407105809,-2.80891125955214,
5.));
#21718=CARTESIAN_POINT('Ctrl Pts',(-1.2457092143346,-2.76008717620201,5.));
#21719=CARTESIAN_POINT('Ctrl Pts',(-1.33140881802392,-2.70693414934569,
5.));
#21720=CARTESIAN_POINT('Ctrl Pts',(-1.4129353161641,-2.65636938639935,5.));
#21721=CARTESIAN_POINT('Ctrl Pts',(-1.49208596169445,-2.60188611256442,
5.));
#21722=CARTESIAN_POINT('Ctrl Pts',(-1.56861084771671,-2.54371537355153,
5.));
#21723=CARTESIAN_POINT('Ctrl Pts',(-1.63557012298619,-2.49281597691525,
5.));
#21724=CARTESIAN_POINT('Ctrl Pts',(-1.70051877227587,-2.43909270266388,
5.));
#21725=CARTESIAN_POINT('Ctrl Pts',(-1.76326584581776,-2.38268809603059,
5.));
#21726=CARTESIAN_POINT('Ctrl Pts',(-1.77895171505325,-2.36858775263627,
5.));
#21727=CARTESIAN_POINT('Ctrl Pts',(-1.79450406853106,-2.35431573679482,
5.));
#21728=CARTESIAN_POINT('Ctrl Pts',(-1.80989576842494,-2.33989703960917,
5.));
#21729=CARTESIAN_POINT('Ctrl Pts',(-1.88231927767376,-2.27205185966276,
5.));
#21730=CARTESIAN_POINT('Ctrl Pts',(-1.95127665379114,-2.20088663840561,
5.));
#21731=CARTESIAN_POINT('Ctrl Pts',(-2.0165263629502,-2.1266887335995,5.));
#21732=CARTESIAN_POINT('Ctrl Pts',(-2.08140824110774,-2.05290910329586,
5.));
#21733=CARTESIAN_POINT('Ctrl Pts',(-2.14262462446156,-1.97613009459816,
5.));
#21734=CARTESIAN_POINT('Ctrl Pts',(-2.19989444056472,-1.89660745904738,
5.));
#21735=CARTESIAN_POINT('Ctrl Pts',(-2.25380452290626,-1.82175001891108,
5.));
#21736=CARTESIAN_POINT('Ctrl Pts',(-2.30421749508371,-1.74446069179507,
5.));
#21737=CARTESIAN_POINT('Ctrl Pts',(-2.35085748563793,-1.66494010874883,
5.));
#21738=CARTESIAN_POINT('Ctrl Pts',(-2.38695950989298,-1.6033866224853,5.));
#21739=CARTESIAN_POINT('Ctrl Pts',(-2.42080014316453,-1.54049593023453,
5.));
#21740=CARTESIAN_POINT('Ctrl Pts',(-2.45223267762586,-1.47635917633043,
5.));
#21741=CARTESIAN_POINT('Ctrl Pts',(-2.45885074786154,-1.46285528460488,
5.));
#21742=CARTESIAN_POINT('Ctrl Pts',(-2.46536230022247,-1.44929534936329,
5.));
#21743=CARTESIAN_POINT('Ctrl Pts',(-2.471759088022,-1.4356951550231,5.));
#21744=CARTESIAN_POINT('Ctrl Pts',(-2.51224453952186,-1.34961913912194,
5.));
#21745=CARTESIAN_POINT('Ctrl Pts',(-2.54820623907542,-1.26179296188141,
5.));
#21746=CARTESIAN_POINT('Ctrl Pts',(-2.57938608018177,-1.17245518793809,
5.));
#21747=CARTESIAN_POINT('Ctrl Pts',(-2.61056592128812,-1.08311741399478,
5.));
#21748=CARTESIAN_POINT('Ctrl Pts',(-2.63696435690728,-0.992267333350395,
5.));
#21749=CARTESIAN_POINT('Ctrl Pts',(-2.65826858221262,-0.900133621000477,
5.));
#21750=CARTESIAN_POINT('Ctrl Pts',(-2.67972778132943,-0.807329698287973,
5.));
#21751=CARTESIAN_POINT('Ctrl Pts',(-2.69601769794397,-0.713222227763925,
5.));
#21752=CARTESIAN_POINT('Ctrl Pts',(-2.70721296581232,-0.618219427263112,
5.));
#21753=CARTESIAN_POINT('Ctrl Pts',(-2.71292220509282,-0.569770946462525,
5.));
#21754=CARTESIAN_POINT('Ctrl Pts',(-2.7173056631566,-0.521089783925043,
5.));
#21755=CARTESIAN_POINT('Ctrl Pts',(-2.7203683315583,-0.472231818984886,
5.));
#21756=CARTESIAN_POINT('Ctrl Pts',(-2.72142997921888,-0.45529562564751,
5.));
#21757=CARTESIAN_POINT('Ctrl Pts',(-2.72233289252141,-0.438338201785387,
5.));
#21758=CARTESIAN_POINT('Ctrl Pts',(-2.72307719183649,-0.421361923846564,
5.));
#21759=CARTESIAN_POINT('Ctrl Pts',(-2.72371459453401,-0.40682378692649,
5.));
#21760=CARTESIAN_POINT('Ctrl Pts',(-2.72423528082335,-0.392280207970546,
5.));
#21761=CARTESIAN_POINT('Ctrl Pts',(-2.72463965223211,-0.3777370307415,5.));
#21762=CARTESIAN_POINT('Ctrl Pts',(-2.7272340736051,-0.284428925823235,
5.));
#21763=CARTESIAN_POINT('Ctrl Pts',(-2.72504745011893,-0.191078680030525,
5.));
#21764=CARTESIAN_POINT('Ctrl Pts',(-2.71820604758435,-0.0980639080872022,
5.));
#21765=CARTESIAN_POINT('Ctrl Pts',(-2.71136148545356,-0.00500617870656192,
5.));
#21766=CARTESIAN_POINT('Ctrl Pts',(-2.69985747016539,0.0877167443723885,
5.));
#21767=CARTESIAN_POINT('Ctrl Pts',(-2.68376992914425,0.179714008003965,
5.));
#21768=CARTESIAN_POINT('Ctrl Pts',(-2.66792655922036,0.27031496919411,5.));
#21769=CARTESIAN_POINT('Ctrl Pts',(-2.64763729016321,0.360212966671102,
5.));
#21770=CARTESIAN_POINT('Ctrl Pts',(-2.62293197139578,0.449008990638608,
5.));
#21771=CARTESIAN_POINT('Ctrl Pts',(-2.61350433154693,0.482893877607947,
5.));
#21772=CARTESIAN_POINT('Ctrl Pts',(-2.60343320797911,0.516617959708256,
5.));
#21773=CARTESIAN_POINT('Ctrl Pts',(-2.5927187899484,0.55015767290499,5.));
#21774=CARTESIAN_POINT('Ctrl Pts',(-2.58640692567121,0.569915919875281,
5.));
#21775=CARTESIAN_POINT('Ctrl Pts',(-2.57987179843875,0.589610167664632,
5.));
#21776=CARTESIAN_POINT('Ctrl Pts',(-2.57311332386527,0.609235450675716,
5.));
#21777=CARTESIAN_POINT('Ctrl Pts',(-2.5676510579122,0.625096798387423,5.));
#21778=CARTESIAN_POINT('Ctrl Pts',(-2.5620452571388,0.640906120496968,5.));
#21779=CARTESIAN_POINT('Ctrl Pts',(-2.55629866051782,0.656654535691256,
5.));
#21780=CARTESIAN_POINT('Ctrl Pts',(-2.52550674415446,0.741039070660769,
5.));
#21781=CARTESIAN_POINT('Ctrl Pts',(-2.4906552842231,0.823736510163055,5.));
#21782=CARTESIAN_POINT('Ctrl Pts',(-2.45179419129016,0.9043762990239,5.));
#21783=CARTESIAN_POINT('Ctrl Pts',(-2.42326911496468,0.963568049912018,
5.));
#21784=CARTESIAN_POINT('Ctrl Pts',(-2.39258278075448,1.0216506842635,5.));
#21785=CARTESIAN_POINT('Ctrl Pts',(-2.35974220291426,1.07846524994913,5.));
#21786=CARTESIAN_POINT('Ctrl Pts',(-2.34707421607123,1.10038100837762,5.));
#21787=CARTESIAN_POINT('Ctrl Pts',(-2.3340855779016,1.12210795474778,5.));
#21788=CARTESIAN_POINT('Ctrl Pts',(-2.32077630204861,1.14363645360599,5.));
#21789=CARTESIAN_POINT('Ctrl Pts',(-2.30811708022228,1.16411345368055,5.));
#21790=CARTESIAN_POINT('Ctrl Pts',(-2.29516494832623,1.18441494534906,5.));
#21791=CARTESIAN_POINT('Ctrl Pts',(-2.28193660666336,1.2045075595742,5.));
#21792=CARTESIAN_POINT('Ctrl Pts',(-2.23464292719215,1.27634223705079,5.));
#21793=CARTESIAN_POINT('Ctrl Pts',(-2.18378817877942,1.34556692931273,5.));
#21794=CARTESIAN_POINT('Ctrl Pts',(-2.12939936247367,1.41182692759809,5.));
#21795=CARTESIAN_POINT('Ctrl Pts',(-2.09060564520546,1.45908796055058,5.));
#21796=CARTESIAN_POINT('Ctrl Pts',(-2.0500132435823,1.504840036578,5.));
#21797=CARTESIAN_POINT('Ctrl Pts',(-2.00762253952656,1.54894112815615,5.));
#21798=CARTESIAN_POINT('Ctrl Pts',(-1.9782483512311,1.57950051132536,5.));
#21799=CARTESIAN_POINT('Ctrl Pts',(-1.94801045703336,1.60926686583501,5.));
#21800=CARTESIAN_POINT('Ctrl Pts',(-1.91694926235925,1.63822229446221,5.));
#21801=CARTESIAN_POINT('Origin',(0.,0.,5.));
#21802=CARTESIAN_POINT('',(2.88675134594813,-5.,5.));
#21803=CARTESIAN_POINT('',(5.77350269189626,0.,5.));
#21804=CARTESIAN_POINT('',(2.88675134594813,-5.,5.));
#21805=CARTESIAN_POINT('',(2.88675134594813,5.,5.));
#21806=CARTESIAN_POINT('',(5.77350269189626,0.,5.));
#21807=CARTESIAN_POINT('',(-2.88675134594813,5.,5.));
#21808=CARTESIAN_POINT('',(2.88675134594813,5.,5.));
#21809=CARTESIAN_POINT('',(-5.77350269189626,1.11022302462516E-15,5.));
#21810=CARTESIAN_POINT('',(-2.88675134594813,5.,5.));
#21811=CARTESIAN_POINT('',(-2.88675134594813,-5.,5.));
#21812=CARTESIAN_POINT('',(-5.77350269189626,7.07050159149938E-16,5.));
#21813=CARTESIAN_POINT('',(-2.88675134594813,-5.,5.));
#21814=CARTESIAN_POINT('Origin',(0.,0.,2.5));
#21815=CARTESIAN_POINT('Origin',(-2.88675134594813,-5.,0.));
#21816=CARTESIAN_POINT('',(-2.88675134594813,-5.,0.));
#21817=CARTESIAN_POINT('',(2.88675134594813,-5.,0.));
#21818=CARTESIAN_POINT('',(-2.88675134594813,-5.,0.));
#21819=CARTESIAN_POINT('',(2.88675134594813,-5.,0.));
#21820=CARTESIAN_POINT('',(-2.88675134594813,-5.,0.));
#21821=CARTESIAN_POINT('Origin',(-5.77350269189626,7.07050159149938E-16,
0.));
#21822=CARTESIAN_POINT('',(-5.77350269189626,7.07050159149938E-16,0.));
#21823=CARTESIAN_POINT('',(-5.77350269189626,7.07050159149938E-16,0.));
#21824=CARTESIAN_POINT('',(-5.77350269189626,7.07050159149938E-16,0.));
#21825=CARTESIAN_POINT('Origin',(-2.88675134594813,5.,0.));
#21826=CARTESIAN_POINT('',(-2.88675134594813,5.,0.));
#21827=CARTESIAN_POINT('',(-2.88675134594813,5.,0.));
#21828=CARTESIAN_POINT('',(-2.88675134594813,5.,0.));
#21829=CARTESIAN_POINT('Origin',(2.88675134594813,5.,0.));
#21830=CARTESIAN_POINT('',(2.88675134594813,5.,0.));
#21831=CARTESIAN_POINT('',(2.88675134594813,5.,0.));
#21832=CARTESIAN_POINT('',(2.88675134594813,5.,0.));
#21833=CARTESIAN_POINT('Origin',(5.77350269189626,0.,0.));
#21834=CARTESIAN_POINT('',(5.77350269189626,0.,0.));
#21835=CARTESIAN_POINT('',(5.77350269189626,0.,0.));
#21836=CARTESIAN_POINT('',(5.77350269189626,0.,0.));
#21837=CARTESIAN_POINT('Origin',(2.88675134594813,-5.,0.));
#21838=CARTESIAN_POINT('',(2.88675134594813,-5.,0.));
#21839=CARTESIAN_POINT('Origin',(0.,0.,0.));
#21840=CARTESIAN_POINT('',(0.,0.,0.));
#21841=CARTESIAN_POINT('',(0.,0.,20.));
#21842=CARTESIAN_POINT('',(0.,0.,23.));
#21843=CARTESIAN_POINT('',(0.,0.,-3.));
#21844=CARTESIAN_POINT('',(-8.,-5.,-6.));
#21845=CARTESIAN_POINT('',(0.,5.,-6.));
#21846=CARTESIAN_POINT('',(-15.,-10.,-3.));
#21847=CARTESIAN_POINT('',(-28.,0.,28.));
#21848=CARTESIAN_POINT('',(-28.,0.,19.));
#21849=CARTESIAN_POINT('',(-28.,0.,14.));
#21850=CARTESIAN_POINT('',(8.,-5.,-6.));
#21851=CARTESIAN_POINT('',(-15.,10.,-3.));
#21852=CARTESIAN_POINT('',(15.,-10.,-3.));
#21853=CARTESIAN_POINT('',(15.,10.,-3.));
#21854=CARTESIAN_POINT('',(28.,0.,28.));
#21855=CARTESIAN_POINT('',(28.,0.,19.));
#21856=CARTESIAN_POINT('',(28.,0.,14.));
#21857=UNCERTAINTY_MEASURE_WITH_UNIT(LENGTH_MEASURE(0.01),#21881,
'DISTANCE_ACCURACY_VALUE',
'Maximum model space distance between geometric entities at asserted c
onnectivities');
#21858=UNCERTAINTY_MEASURE_WITH_UNIT(LENGTH_MEASURE(0.01),#21881,
'DISTANCE_ACCURACY_VALUE',
'Maximum model space distance between geometric entities at asserted c
onnectivities');
#21859=UNCERTAINTY_MEASURE_WITH_UNIT(LENGTH_MEASURE(0.01),#21881,
'DISTANCE_ACCURACY_VALUE',
'Maximum model space distance between geometric entities at asserted c
onnectivities');
#21860=UNCERTAINTY_MEASURE_WITH_UNIT(LENGTH_MEASURE(0.01),#21881,
'DISTANCE_ACCURACY_VALUE',
'Maximum model space distance between geometric entities at asserted c
onnectivities');
#21861=UNCERTAINTY_MEASURE_WITH_UNIT(LENGTH_MEASURE(0.01),#21881,
'DISTANCE_ACCURACY_VALUE',
'Maximum model space distance between geometric entities at asserted c
onnectivities');
#21862=UNCERTAINTY_MEASURE_WITH_UNIT(LENGTH_MEASURE(0.01),#21881,
'DISTANCE_ACCURACY_VALUE',
'Maximum model space distance between geometric entities at asserted c
onnectivities');
#21863=UNCERTAINTY_MEASURE_WITH_UNIT(LENGTH_MEASURE(0.01),#21881,
'DISTANCE_ACCURACY_VALUE',
'Maximum model space distance between geometric entities at asserted c
onnectivities');
#21864=UNCERTAINTY_MEASURE_WITH_UNIT(LENGTH_MEASURE(0.01),#21881,
'DISTANCE_ACCURACY_VALUE',
'Maximum model space distance between geometric entities at asserted c
onnectivities');
#21865=UNCERTAINTY_MEASURE_WITH_UNIT(LENGTH_MEASURE(0.01),#21881,
'DISTANCE_ACCURACY_VALUE',
'Maximum model space distance between geometric entities at asserted c
onnectivities');
#21866=UNCERTAINTY_MEASURE_WITH_UNIT(LENGTH_MEASURE(0.01),#21881,
'DISTANCE_ACCURACY_VALUE',
'Maximum model space distance between geometric entities at asserted c
onnectivities');
#21867=UNCERTAINTY_MEASURE_WITH_UNIT(LENGTH_MEASURE(0.01),#21881,
'DISTANCE_ACCURACY_VALUE',
'Maximum model space distance between geometric entities at asserted c
onnectivities');
#21868=UNCERTAINTY_MEASURE_WITH_UNIT(LENGTH_MEASURE(0.01),#21881,
'DISTANCE_ACCURACY_VALUE',
'Maximum model space distance between geometric entities at asserted c
onnectivities');
#21869=(
GEOMETRIC_REPRESENTATION_CONTEXT(3)
GLOBAL_UNCERTAINTY_ASSIGNED_CONTEXT((#21857))
GLOBAL_UNIT_ASSIGNED_CONTEXT((#21881,#21883,#21884))
REPRESENTATION_CONTEXT('','3D')
);
#21870=(
GEOMETRIC_REPRESENTATION_CONTEXT(3)
GLOBAL_UNCERTAINTY_ASSIGNED_CONTEXT((#21858))
GLOBAL_UNIT_ASSIGNED_CONTEXT((#21881,#21883,#21884))
REPRESENTATION_CONTEXT('','3D')
);
#21871=(
GEOMETRIC_REPRESENTATION_CONTEXT(3)
GLOBAL_UNCERTAINTY_ASSIGNED_CONTEXT((#21859))
GLOBAL_UNIT_ASSIGNED_CONTEXT((#21881,#21883,#21884))
REPRESENTATION_CONTEXT('','3D')
);
#21872=(
GEOMETRIC_REPRESENTATION_CONTEXT(3)
GLOBAL_UNCERTAINTY_ASSIGNED_CONTEXT((#21860))
GLOBAL_UNIT_ASSIGNED_CONTEXT((#21881,#21883,#21884))
REPRESENTATION_CONTEXT('','3D')
);
#21873=(
GEOMETRIC_REPRESENTATION_CONTEXT(3)
GLOBAL_UNCERTAINTY_ASSIGNED_CONTEXT((#21861))
GLOBAL_UNIT_ASSIGNED_CONTEXT((#21881,#21883,#21884))
REPRESENTATION_CONTEXT('','3D')
);
#21874=(
GEOMETRIC_REPRESENTATION_CONTEXT(3)
GLOBAL_UNCERTAINTY_ASSIGNED_CONTEXT((#21862))
GLOBAL_UNIT_ASSIGNED_CONTEXT((#21881,#21883,#21884))
REPRESENTATION_CONTEXT('','3D')
);
#21875=(
GEOMETRIC_REPRESENTATION_CONTEXT(3)
GLOBAL_UNCERTAINTY_ASSIGNED_CONTEXT((#21863))
GLOBAL_UNIT_ASSIGNED_CONTEXT((#21881,#21883,#21884))
REPRESENTATION_CONTEXT('','3D')
);
#21876=(
GEOMETRIC_REPRESENTATION_CONTEXT(3)
GLOBAL_UNCERTAINTY_ASSIGNED_CONTEXT((#21864))
GLOBAL_UNIT_ASSIGNED_CONTEXT((#21881,#21883,#21884))
REPRESENTATION_CONTEXT('','3D')
);
#21877=(
GEOMETRIC_REPRESENTATION_CONTEXT(3)
GLOBAL_UNCERTAINTY_ASSIGNED_CONTEXT((#21865))
GLOBAL_UNIT_ASSIGNED_CONTEXT((#21881,#21883,#21884))
REPRESENTATION_CONTEXT('','3D')
);
#21878=(
GEOMETRIC_REPRESENTATION_CONTEXT(3)
GLOBAL_UNCERTAINTY_ASSIGNED_CONTEXT((#21866))
GLOBAL_UNIT_ASSIGNED_CONTEXT((#21881,#21883,#21884))
REPRESENTATION_CONTEXT('','3D')
);
#21879=(
GEOMETRIC_REPRESENTATION_CONTEXT(3)
GLOBAL_UNCERTAINTY_ASSIGNED_CONTEXT((#21867))
GLOBAL_UNIT_ASSIGNED_CONTEXT((#21881,#21883,#21884))
REPRESENTATION_CONTEXT('','3D')
);
#21880=(
GEOMETRIC_REPRESENTATION_CONTEXT(3)
GLOBAL_UNCERTAINTY_ASSIGNED_CONTEXT((#21868))
GLOBAL_UNIT_ASSIGNED_CONTEXT((#21881,#21883,#21884))
REPRESENTATION_CONTEXT('','3D')
);
#21881=(
LENGTH_UNIT()
NAMED_UNIT(*)
SI_UNIT(.MILLI.,.METRE.)
);
#21882=(
LENGTH_UNIT()
NAMED_UNIT(*)
SI_UNIT($,.METRE.)
);
#21883=(
NAMED_UNIT(*)
PLANE_ANGLE_UNIT()
SI_UNIT($,.RADIAN.)
);
#21884=(
NAMED_UNIT(*)
SI_UNIT($,.STERADIAN.)
SOLID_ANGLE_UNIT()
);
#21885=SHAPE_DEFINITION_REPRESENTATION(#21896,#21924);
#21886=SHAPE_DEFINITION_REPRESENTATION(#21897,#21925);
#21887=SHAPE_DEFINITION_REPRESENTATION(#21898,#21926);
#21888=SHAPE_DEFINITION_REPRESENTATION(#21899,#21927);
#21889=SHAPE_DEFINITION_REPRESENTATION(#21900,#21928);
#21890=SHAPE_DEFINITION_REPRESENTATION(#21901,#21929);
#21891=SHAPE_DEFINITION_REPRESENTATION(#21902,#21930);
#21892=SHAPE_DEFINITION_REPRESENTATION(#21903,#21931);
#21893=SHAPE_DEFINITION_REPRESENTATION(#21904,#21932);
#21894=SHAPE_DEFINITION_REPRESENTATION(#21905,#21933);
#21895=SHAPE_DEFINITION_REPRESENTATION(#21906,#21934);
#21896=PRODUCT_DEFINITION_SHAPE('',$,#21936);
#21897=PRODUCT_DEFINITION_SHAPE('',$,#21937);
#21898=PRODUCT_DEFINITION_SHAPE('',$,#21938);
#21899=PRODUCT_DEFINITION_SHAPE('',$,#21939);
#21900=PRODUCT_DEFINITION_SHAPE('',$,#21940);
#21901=PRODUCT_DEFINITION_SHAPE('',$,#21941);
#21902=PRODUCT_DEFINITION_SHAPE('',$,#21942);
#21903=PRODUCT_DEFINITION_SHAPE('',$,#21943);
#21904=PRODUCT_DEFINITION_SHAPE('',$,#21944);
#21905=PRODUCT_DEFINITION_SHAPE('',$,#21945);
#21906=PRODUCT_DEFINITION_SHAPE('',$,#21946);
#21907=PRODUCT_DEFINITION_SHAPE($,$,#62);
#21908=PRODUCT_DEFINITION_SHAPE($,$,#63);
#21909=PRODUCT_DEFINITION_SHAPE($,$,#64);
#21910=PRODUCT_DEFINITION_SHAPE($,$,#65);
#21911=PRODUCT_DEFINITION_SHAPE($,$,#66);
#21912=PRODUCT_DEFINITION_SHAPE($,$,#67);
#21913=PRODUCT_DEFINITION_SHAPE($,$,#68);
#21914=PRODUCT_DEFINITION_SHAPE($,$,#69);
#21915=PRODUCT_DEFINITION_SHAPE($,$,#70);
#21916=PRODUCT_DEFINITION_SHAPE($,$,#71);
#21917=PRODUCT_DEFINITION_SHAPE($,$,#72);
#21918=PRODUCT_DEFINITION_SHAPE($,$,#73);
#21919=PRODUCT_DEFINITION_SHAPE($,$,#74);
#21920=PRODUCT_DEFINITION_SHAPE($,$,#75);
#21921=PRODUCT_DEFINITION_SHAPE($,$,#76);
#21922=PRODUCT_DEFINITION_SHAPE($,$,#77);
#21923=PRODUCT_DEFINITION_SHAPE($,$,#78);
#21924=SHAPE_REPRESENTATION('',(#6502,#6950,#6951,#6952,#6953,#6954,#6955,
#6956,#6957,#6958,#6959,#6960,#6961,#6962,#6963,#6964,#6965,#6966),#21869);
#21925=SHAPE_REPRESENTATION('',(#6503),#21870);
#21926=SHAPE_REPRESENTATION('',(#6693),#21871);
#21927=SHAPE_REPRESENTATION('',(#6754),#21872);
#21928=SHAPE_REPRESENTATION('',(#6771),#21873);
#21929=SHAPE_REPRESENTATION('',(#6802),#21874);
#21930=SHAPE_REPRESENTATION('',(#6812),#21875);
#21931=SHAPE_REPRESENTATION('',(#6822),#21876);
#21932=SHAPE_REPRESENTATION('',(#6864),#21877);
#21933=SHAPE_REPRESENTATION('',(#6916),#21878);
#21934=SHAPE_REPRESENTATION('',(#6925),#21879);
#21935=PRODUCT_DEFINITION_CONTEXT('part definition',#21970,'design');
#21936=PRODUCT_DEFINITION('MAS-646','MAS-646',#21947,#21935);
#21937=PRODUCT_DEFINITION('Inlet housing','Inlet housing',#21948,#21935);
#21938=PRODUCT_DEFINITION('Panel plate','Panel plate',#21949,#21935);
#21939=PRODUCT_DEFINITION('Flange gasket','Flange gasket',#21950,#21935);
#21940=PRODUCT_DEFINITION('Contact retaining plate',
'Contact retaining plate',#21951,#21935);
#21941=PRODUCT_DEFINITION('Ground contact','Ground contact',#21952,#21935);
#21942=PRODUCT_DEFINITION('Line contact','Line contact',#21953,#21935);
#21943=PRODUCT_DEFINITION('Socket head cap screw M4x8',
'Socket head cap screw M4x8',#21954,#21935);
#21944=PRODUCT_DEFINITION('Socket head cap screw M6x16',
'Socket head cap screw M6x16',#21955,#21935);
#21945=PRODUCT_DEFINITION('Flat washer M6','Flat washer M6',#21956,#21935);
#21946=PRODUCT_DEFINITION('Hex nut M6','Hex nut M6',#21957,#21935);
#21947=PRODUCT_DEFINITION_FORMATION('',$,#21972);
#21948=PRODUCT_DEFINITION_FORMATION('',$,#21973);
#21949=PRODUCT_DEFINITION_FORMATION('',$,#21974);
#21950=PRODUCT_DEFINITION_FORMATION('',$,#21975);
#21951=PRODUCT_DEFINITION_FORMATION('',$,#21976);
#21952=PRODUCT_DEFINITION_FORMATION('',$,#21977);
#21953=PRODUCT_DEFINITION_FORMATION('',$,#21978);
#21954=PRODUCT_DEFINITION_FORMATION('',$,#21979);
#21955=PRODUCT_DEFINITION_FORMATION('',$,#21980);
#21956=PRODUCT_DEFINITION_FORMATION('',$,#21981);
#21957=PRODUCT_DEFINITION_FORMATION('',$,#21982);
#21958=PRODUCT_RELATED_PRODUCT_CATEGORY('MAS-646','MAS-646',(#21972));
#21959=PRODUCT_RELATED_PRODUCT_CATEGORY('Inlet housing','Inlet housing',
(#21973));
#21960=PRODUCT_RELATED_PRODUCT_CATEGORY('Panel plate','Panel plate',(#21974));
#21961=PRODUCT_RELATED_PRODUCT_CATEGORY('Flange gasket','Flange gasket',
(#21975));
#21962=PRODUCT_RELATED_PRODUCT_CATEGORY('Contact retaining plate',
'Contact retaining plate',(#21976));
#21963=PRODUCT_RELATED_PRODUCT_CATEGORY('Ground contact',
'Ground contact',(#21977));
#21964=PRODUCT_RELATED_PRODUCT_CATEGORY('Line contact','Line contact',(#21978));
#21965=PRODUCT_RELATED_PRODUCT_CATEGORY('Socket head cap screw M4x8',
'Socket head cap screw M4x8',(#21979));
#21966=PRODUCT_RELATED_PRODUCT_CATEGORY('Socket head cap screw M6x16',
'Socket head cap screw M6x16',(#21980));
#21967=PRODUCT_RELATED_PRODUCT_CATEGORY('Flat washer M6',
'Flat washer M6',(#21981));
#21968=PRODUCT_RELATED_PRODUCT_CATEGORY('Hex nut M6','Hex nut M6',(#21982));
#21969=APPLICATION_PROTOCOL_DEFINITION('international standard',
'automotive_design',2009,#21970);
#21970=APPLICATION_CONTEXT(
'Core Data for Automotive Mechanical Design Process');
#21971=PRODUCT_CONTEXT('part definition',#21970,'mechanical');
#21972=PRODUCT('MAS-646','MAS-646',
'Independent keyed three-contact power inlet for the IEC-connector des
ign category. Longer ground blade, retained contacts, wire termination
 holes and sealed bolted panel interface. Nominal custom interface; IE
C dimensional compatibility and electrical ratings are not assigned.',(#21971));
#21973=PRODUCT('Inlet housing','Inlet housing',$,(#21971));
#21974=PRODUCT('Panel plate','Panel plate',$,(#21971));
#21975=PRODUCT('Flange gasket','Flange gasket',$,(#21971));
#21976=PRODUCT('Contact retaining plate','Contact retaining plate',$,(#21971));
#21977=PRODUCT('Ground contact','Ground contact',$,(#21971));
#21978=PRODUCT('Line contact','Line contact',$,(#21971));
#21979=PRODUCT('Socket head cap screw M4x8',
'Socket head cap screw M4x8',$,(#21971));
#21980=PRODUCT('Socket head cap screw M6x16',
'Socket head cap screw M6x16',$,(#21971));
#21981=PRODUCT('Flat washer M6','Flat washer M6',$,(#21971));
#21982=PRODUCT('Hex nut M6','Hex nut M6',$,(#21971));
#21983=PRESENTATION_STYLE_ASSIGNMENT((#21989));
#21984=PRESENTATION_STYLE_ASSIGNMENT((#21990));
#21985=PRESENTATION_STYLE_ASSIGNMENT((#21991));
#21986=PRESENTATION_STYLE_ASSIGNMENT((#21992));
#21987=PRESENTATION_STYLE_ASSIGNMENT((#21993));
#21988=PRESENTATION_STYLE_ASSIGNMENT((#21994));
#21989=SURFACE_STYLE_USAGE(.BOTH.,#21995);
#21990=SURFACE_STYLE_USAGE(.BOTH.,#21996);
#21991=SURFACE_STYLE_USAGE(.BOTH.,#21997);
#21992=SURFACE_STYLE_USAGE(.BOTH.,#21998);
#21993=SURFACE_STYLE_USAGE(.BOTH.,#21999);
#21994=SURFACE_STYLE_USAGE(.BOTH.,#22000);
#21995=SURFACE_SIDE_STYLE('',(#22001));
#21996=SURFACE_SIDE_STYLE('',(#22002));
#21997=SURFACE_SIDE_STYLE('',(#22003));
#21998=SURFACE_SIDE_STYLE('',(#22004));
#21999=SURFACE_SIDE_STYLE('',(#22005));
#22000=SURFACE_SIDE_STYLE('',(#22006));
#22001=SURFACE_STYLE_FILL_AREA(#22007);
#22002=SURFACE_STYLE_FILL_AREA(#22008);
#22003=SURFACE_STYLE_FILL_AREA(#22009);
#22004=SURFACE_STYLE_FILL_AREA(#22010);
#22005=SURFACE_STYLE_FILL_AREA(#22011);
#22006=SURFACE_STYLE_FILL_AREA(#22012);
#22007=FILL_AREA_STYLE('Steel - Satin',(#22013));
#22008=FILL_AREA_STYLE('Dark blue',(#22014));
#22009=FILL_AREA_STYLE('Gray',(#22015));
#22010=FILL_AREA_STYLE('Dark gray',(#22016));
#22011=FILL_AREA_STYLE('Sky blue',(#22017));
#22012=FILL_AREA_STYLE('Light gray',(#22018));
#22013=FILL_AREA_STYLE_COLOUR('Steel - Satin',#22019);
#22014=FILL_AREA_STYLE_COLOUR('Dark blue',#22020);
#22015=FILL_AREA_STYLE_COLOUR('Gray',#22021);
#22016=FILL_AREA_STYLE_COLOUR('Dark gray',#22022);
#22017=FILL_AREA_STYLE_COLOUR('Sky blue',#22023);
#22018=FILL_AREA_STYLE_COLOUR('Light gray',#22024);
#22019=COLOUR_RGB('Steel - Satin',0.627450980392157,0.627450980392157,0.627450980392157);
#22020=COLOUR_RGB('Dark blue',0.0901960784313725,0.270588235294118,0.513725490196078);
#22021=COLOUR_RGB('Gray',0.407843137254902,0.447058823529412,0.498039215686275);
#22022=COLOUR_RGB('Dark gray',0.250980392156863,0.282352941176471,0.32156862745098);
#22023=COLOUR_RGB('Sky blue',0.317647058823529,0.686274509803922,0.890196078431372);
#22024=COLOUR_RGB('Light gray',0.725490196078431,0.752941176470588,0.792156862745098);
ENDSEC;
END-ISO-10303-21;
